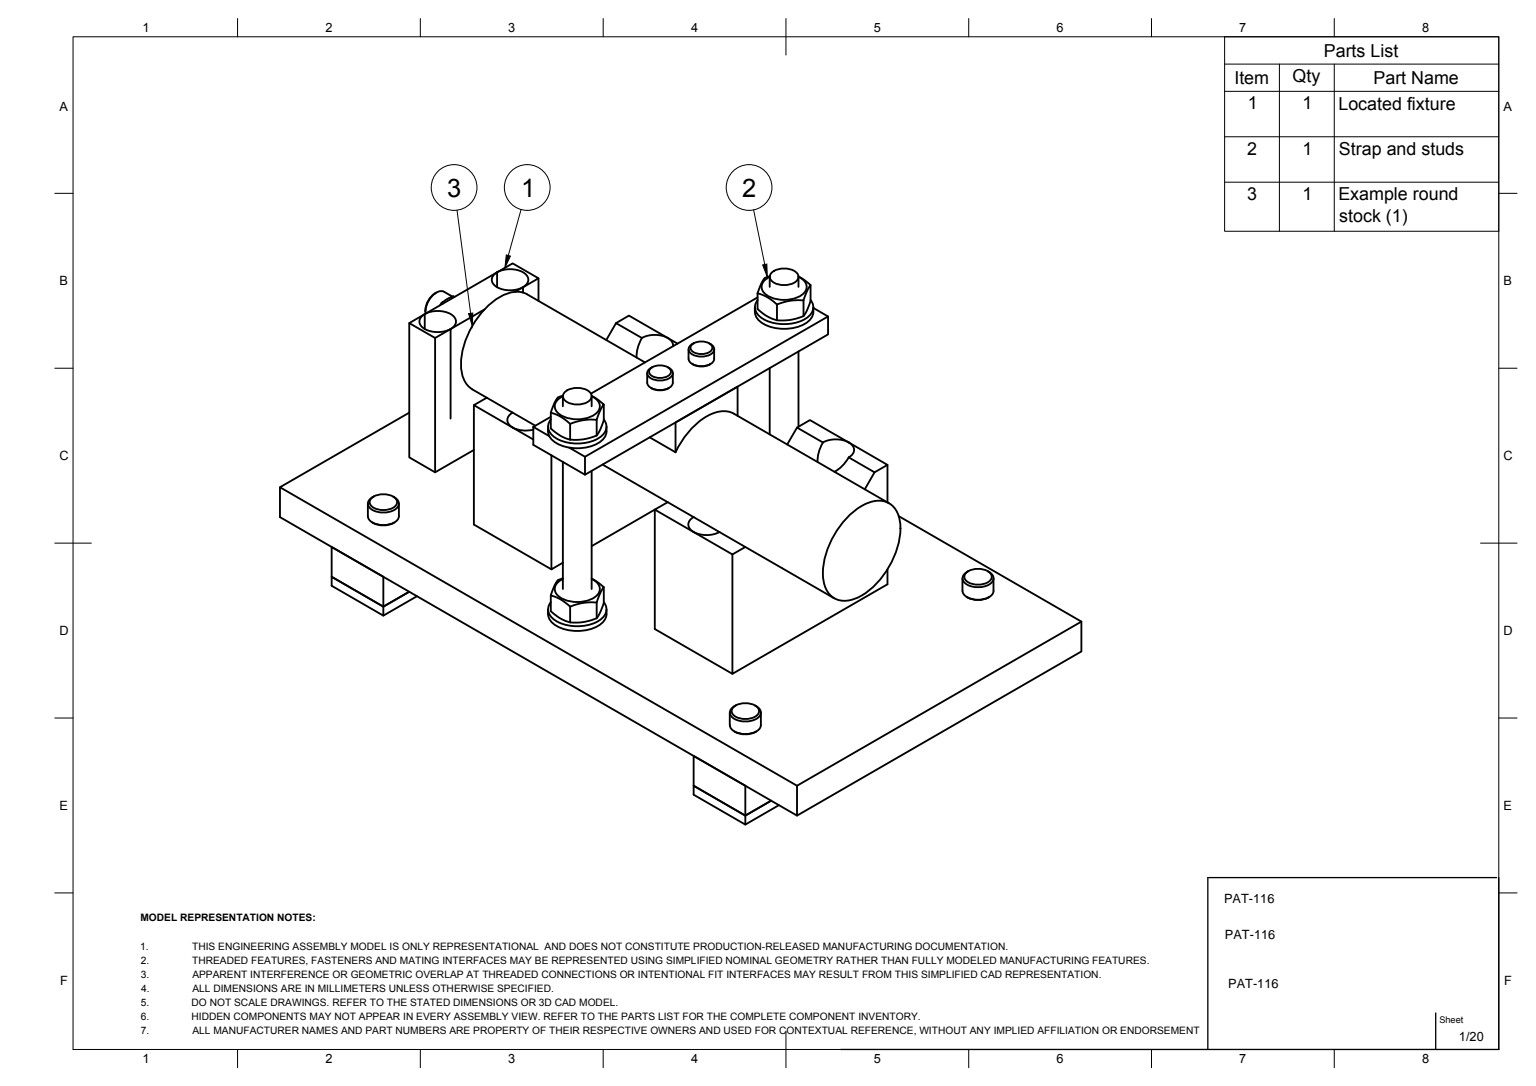
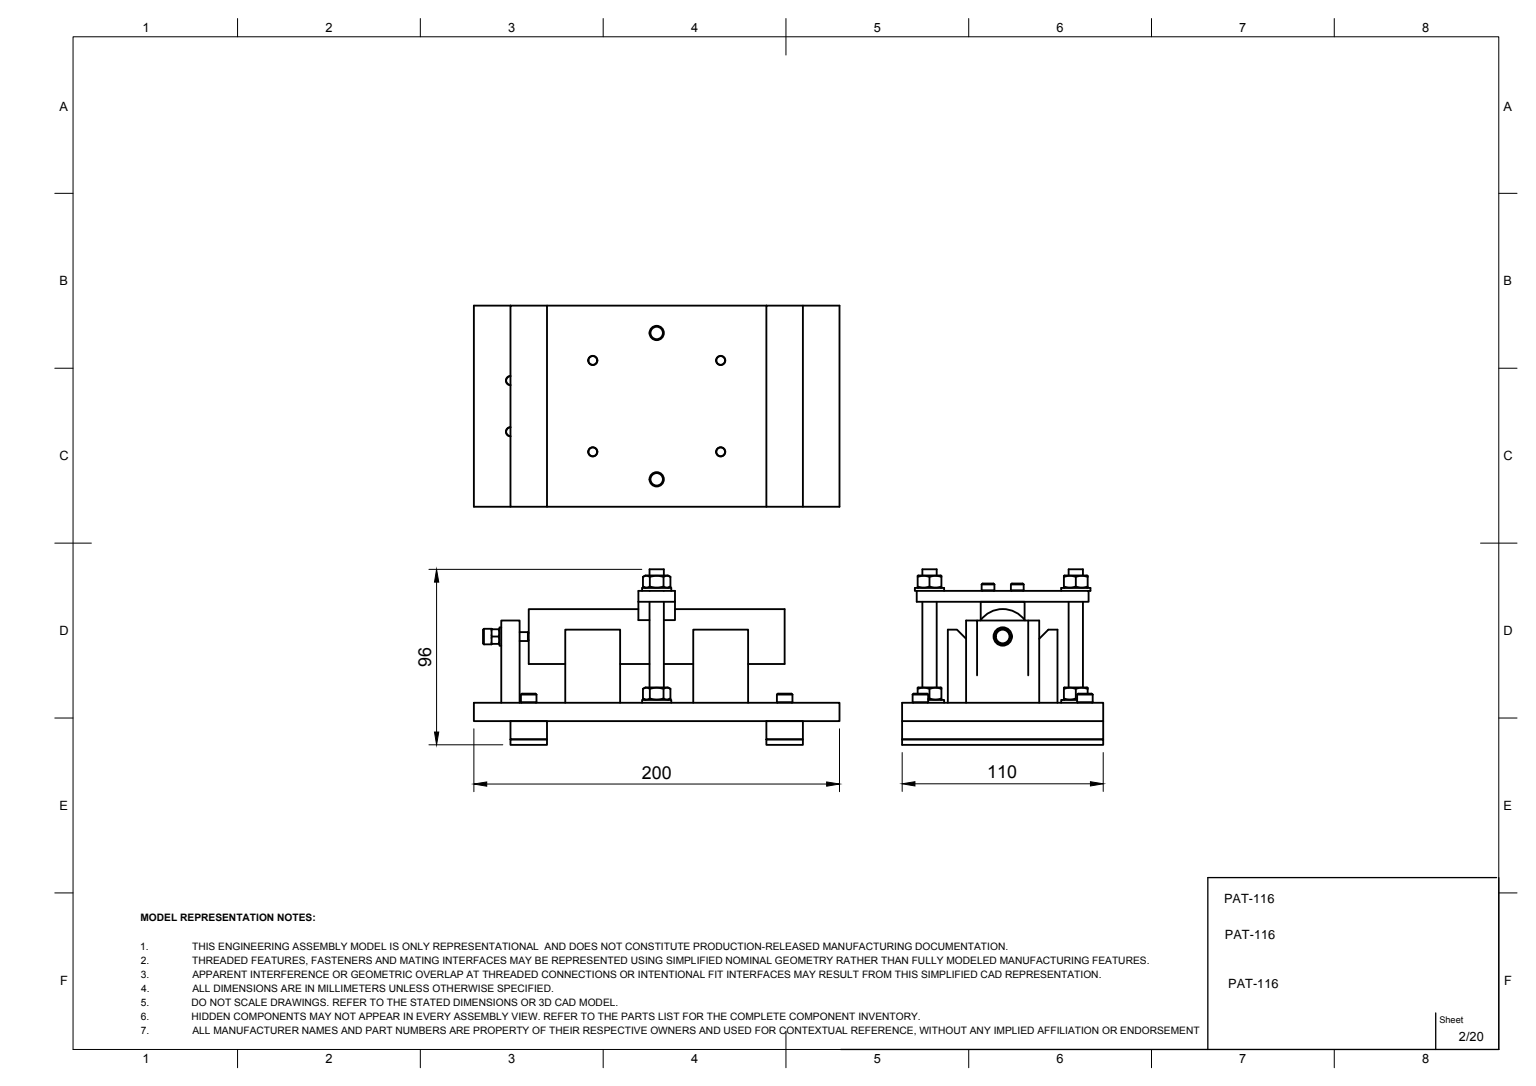
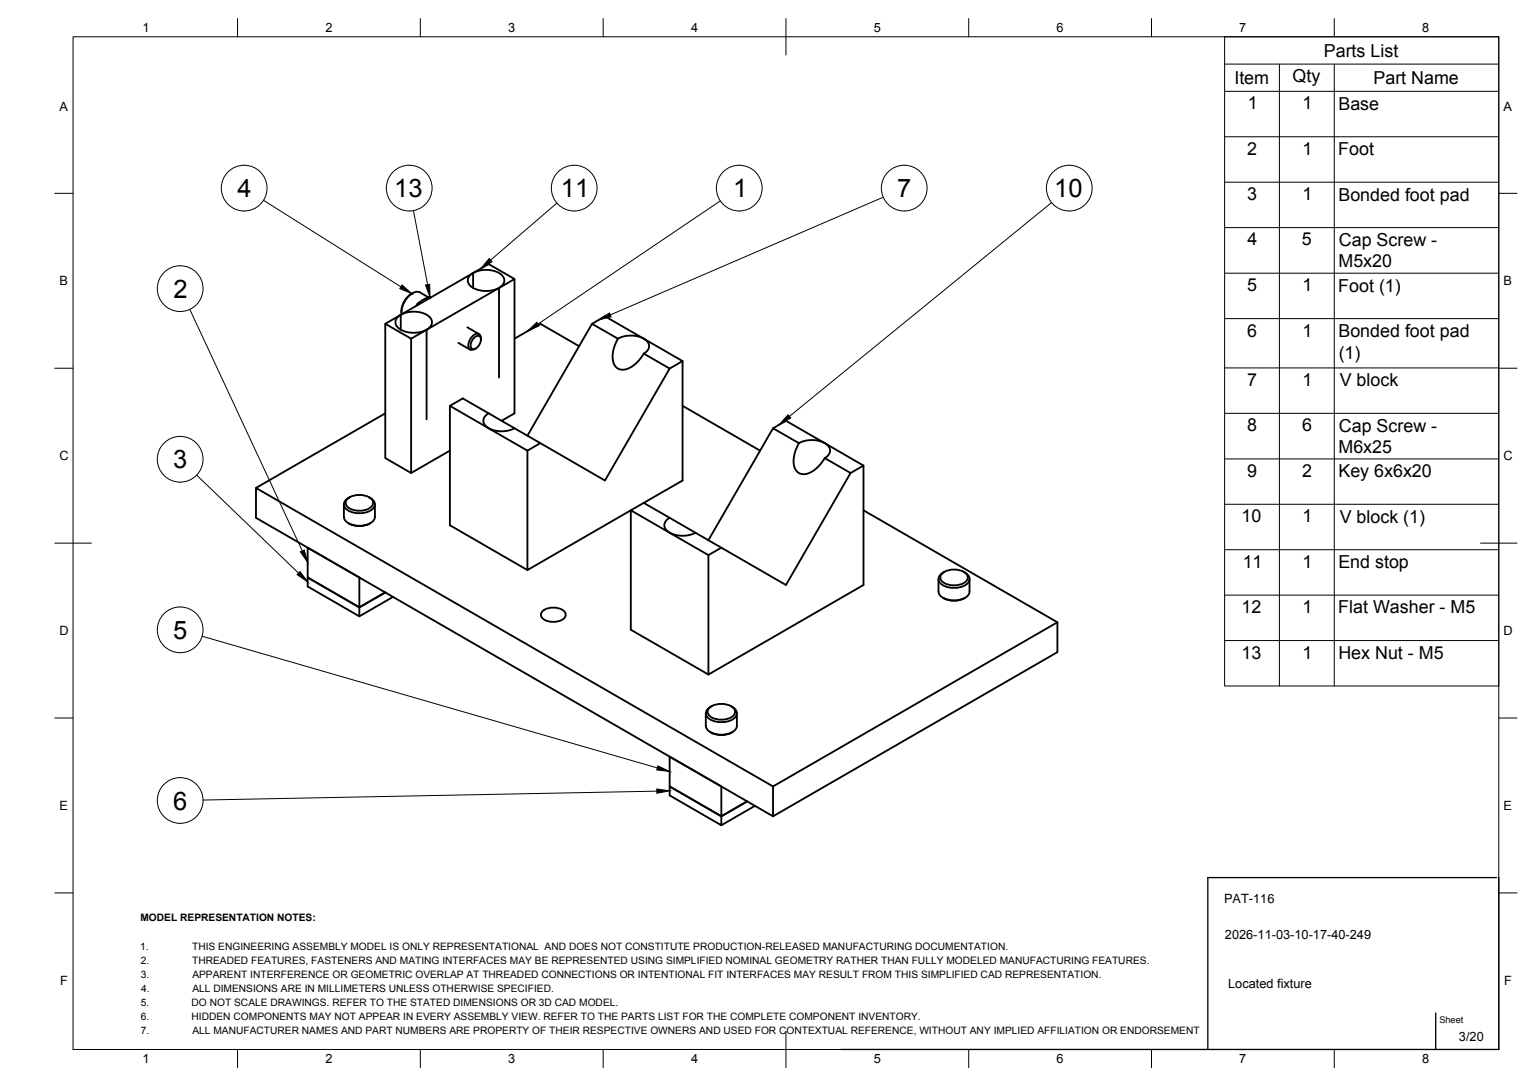
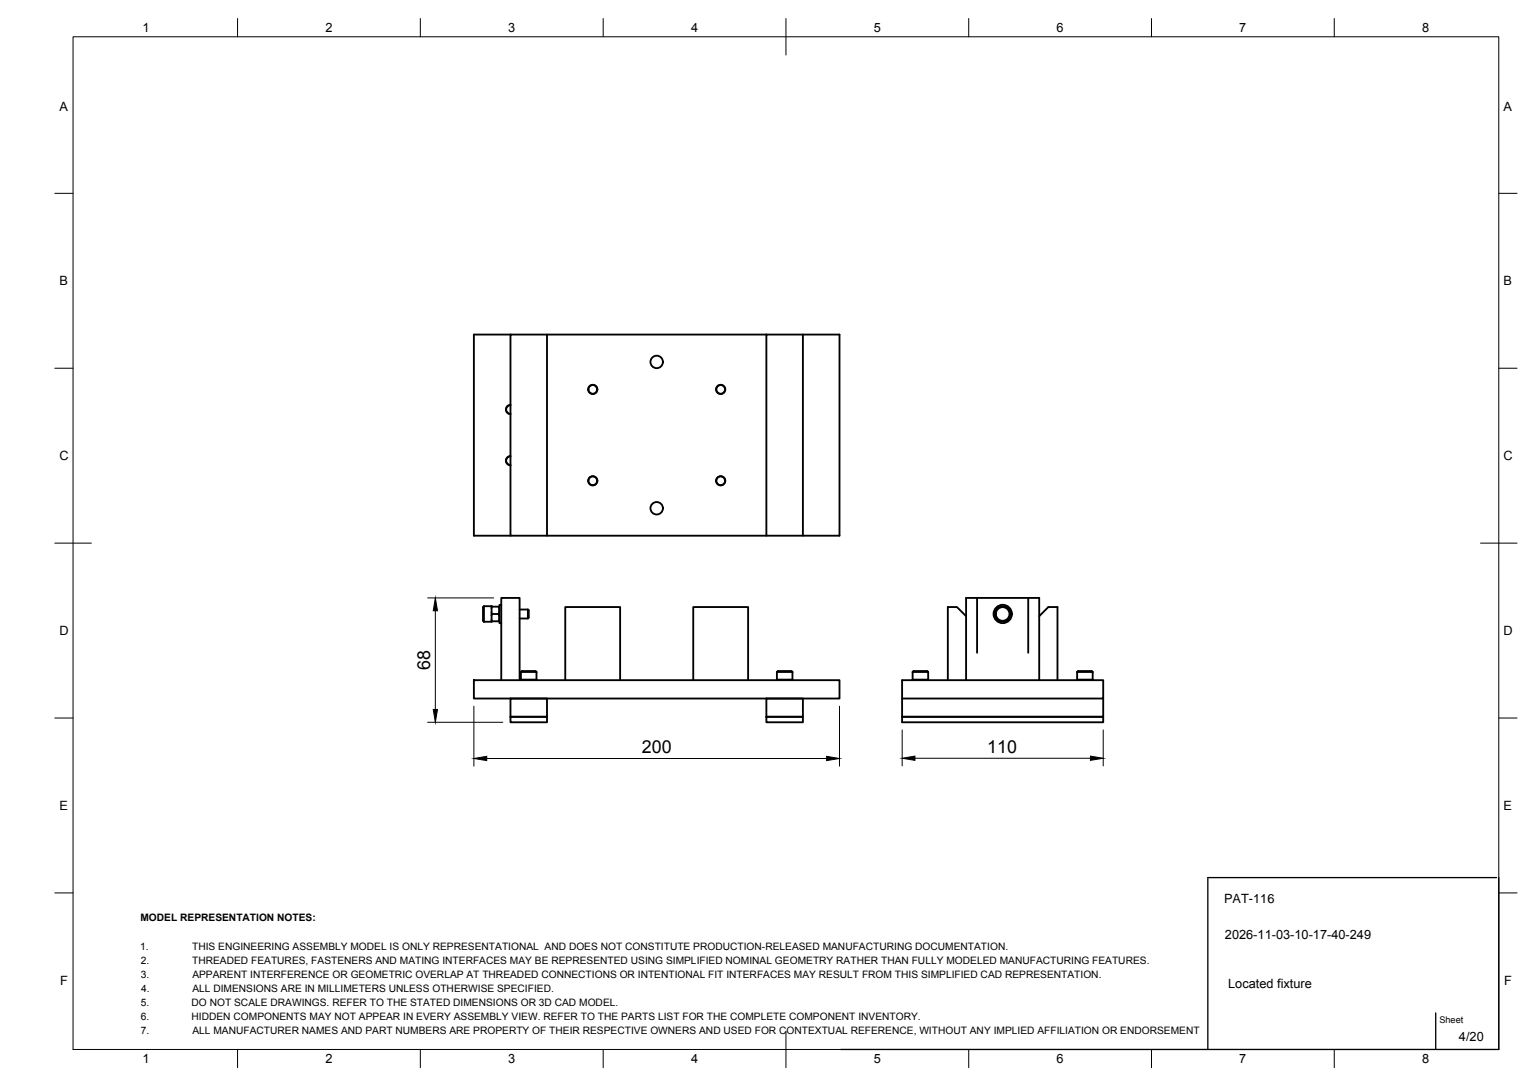
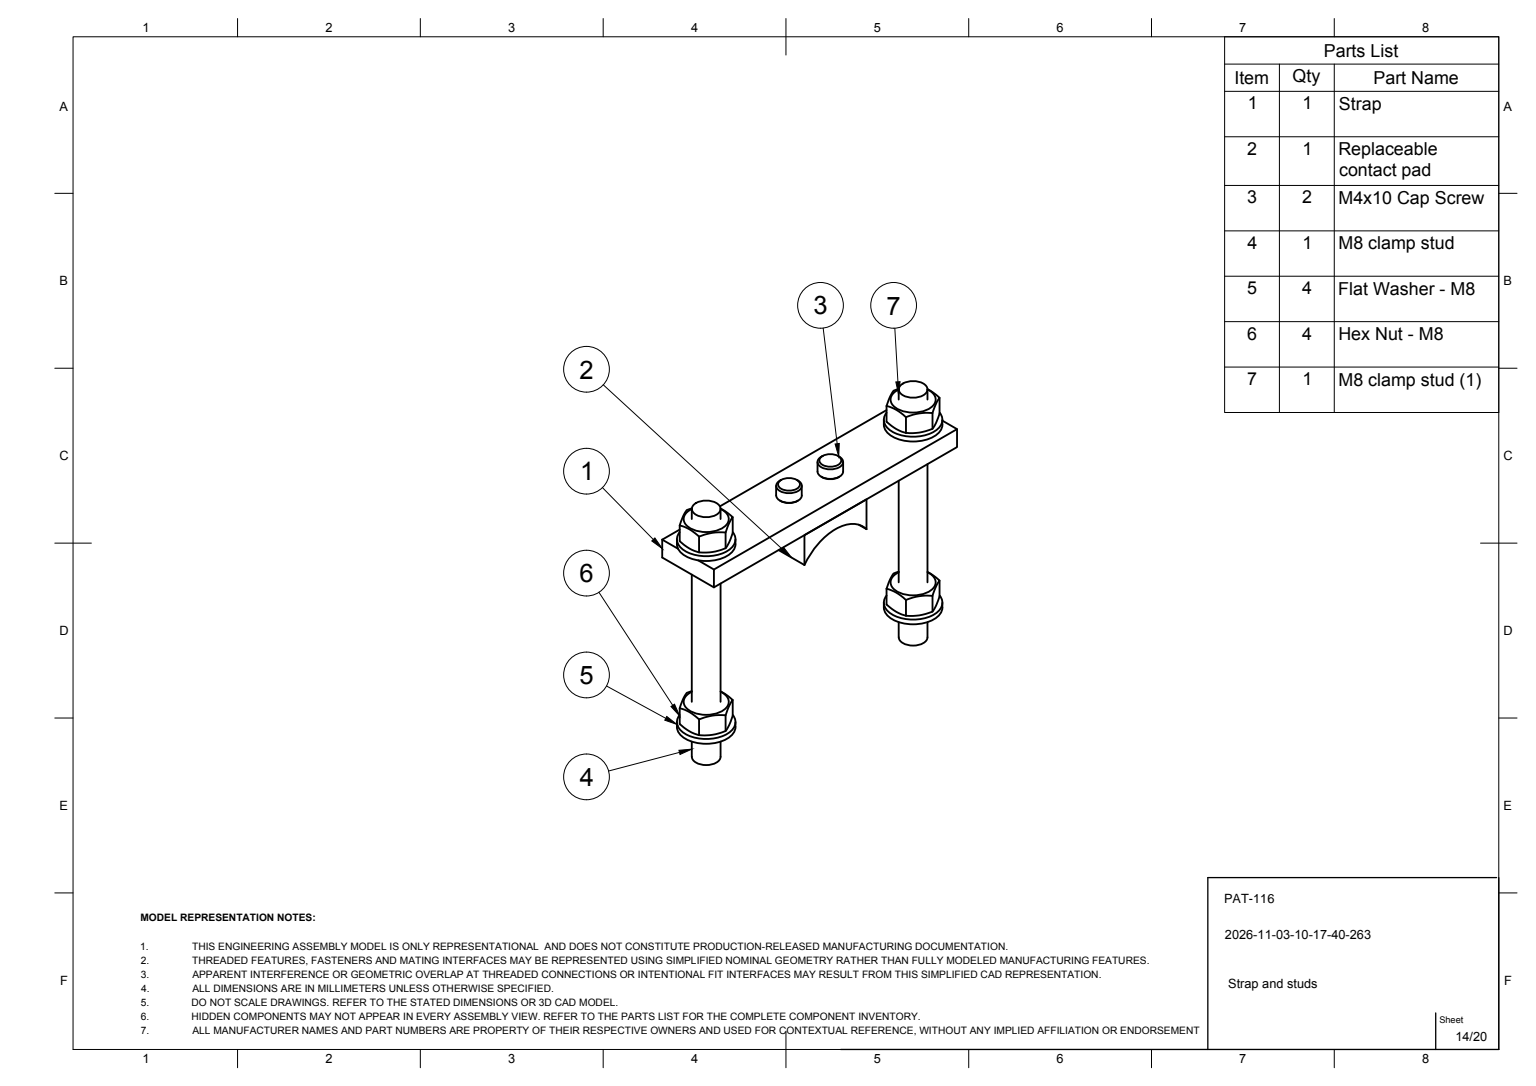
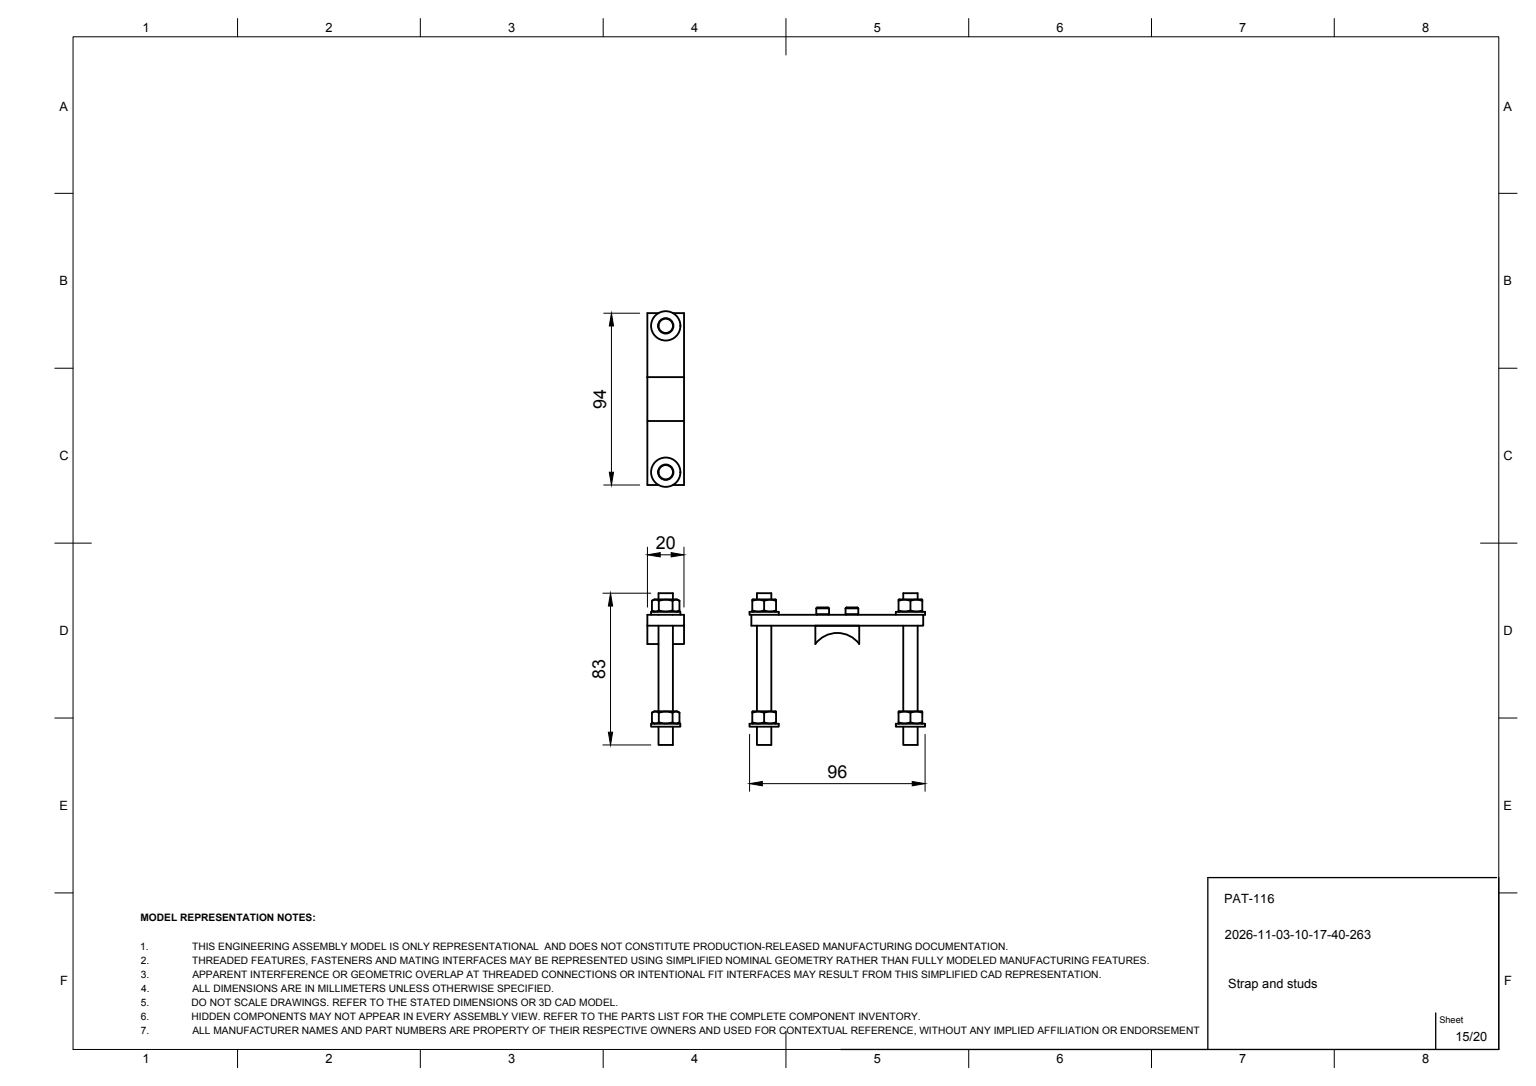
ISO-10303-21;
HEADER;
/* Generated by software containing ST-Developer
 * from STEP Tools, Inc. (www.steptools.com) 
 */

FILE_DESCRIPTION(
/* description */ ('V-block with clamp strap'),
/* implementation_level */ '2;1');

FILE_NAME(
/* name */ 'PAT-116',
/* time_stamp */ '2026-10-27T10:50:53-07:00',
/* author */ (''),
/* organization */ (''),
/* preprocessor_version */ 'ST-DEVELOPER v20.2',
/* originating_system */ 'Autodesk Translation Framework v15.17.0.0',
/* authorisation */ '');

FILE_SCHEMA (('AUTOMOTIVE_DESIGN { 1 0 10303 214 3 1 1 }'));
ENDSEC;

DATA;
#10=MECHANICAL_DESIGN_GEOMETRIC_PRESENTATION_REPRESENTATION('',(#266,#267,
#268,#269,#270,#271,#272,#273,#274,#275,#276,#277,#278,#279,#280,#281,#282,
#283,#284,#285,#286),#7344);
#11=ITEM_DEFINED_TRANSFORMATION($,$,#4406,#4697);
#12=ITEM_DEFINED_TRANSFORMATION($,$,#4459,#4698);
#13=ITEM_DEFINED_TRANSFORMATION($,$,#4472,#4699);
#14=ITEM_DEFINED_TRANSFORMATION($,$,#4479,#4700);
#15=ITEM_DEFINED_TRANSFORMATION($,$,#4492,#4701);
#16=ITEM_DEFINED_TRANSFORMATION($,$,#4499,#4702);
#17=ITEM_DEFINED_TRANSFORMATION($,$,#4538,#4703);
#18=ITEM_DEFINED_TRANSFORMATION($,$,#4577,#4704);
#19=ITEM_DEFINED_TRANSFORMATION($,$,#4646,#4705);
#20=ITEM_DEFINED_TRANSFORMATION($,$,#4646,#4706);
#21=ITEM_DEFINED_TRANSFORMATION($,$,#4646,#4707);
#22=ITEM_DEFINED_TRANSFORMATION($,$,#4646,#4708);
#23=ITEM_DEFINED_TRANSFORMATION($,$,#4620,#4709);
#24=ITEM_DEFINED_TRANSFORMATION($,$,#4620,#4710);
#25=ITEM_DEFINED_TRANSFORMATION($,$,#4609,#4711);
#26=ITEM_DEFINED_TRANSFORMATION($,$,#4620,#4712);
#27=ITEM_DEFINED_TRANSFORMATION($,$,#4620,#4713);
#28=ITEM_DEFINED_TRANSFORMATION($,$,#4609,#4714);
#29=ITEM_DEFINED_TRANSFORMATION($,$,#4620,#4715);
#30=ITEM_DEFINED_TRANSFORMATION($,$,#4620,#4716);
#31=ITEM_DEFINED_TRANSFORMATION($,$,#4646,#4717);
#32=ITEM_DEFINED_TRANSFORMATION($,$,#4672,#4718);
#33=ITEM_DEFINED_TRANSFORMATION($,$,#4681,#4719);
#34=ITEM_DEFINED_TRANSFORMATION($,$,#4721,#4818);
#35=ITEM_DEFINED_TRANSFORMATION($,$,#4740,#4819);
#36=ITEM_DEFINED_TRANSFORMATION($,$,#4757,#4820);
#37=ITEM_DEFINED_TRANSFORMATION($,$,#4763,#4821);
#38=ITEM_DEFINED_TRANSFORMATION($,$,#4769,#4822);
#39=ITEM_DEFINED_TRANSFORMATION($,$,#4769,#4823);
#40=ITEM_DEFINED_TRANSFORMATION($,$,#4793,#4824);
#41=ITEM_DEFINED_TRANSFORMATION($,$,#4802,#4825);
#42=ITEM_DEFINED_TRANSFORMATION($,$,#4793,#4826);
#43=ITEM_DEFINED_TRANSFORMATION($,$,#4802,#4827);
#44=ITEM_DEFINED_TRANSFORMATION($,$,#4793,#4828);
#45=ITEM_DEFINED_TRANSFORMATION($,$,#4802,#4829);
#46=ITEM_DEFINED_TRANSFORMATION($,$,#4793,#4830);
#47=ITEM_DEFINED_TRANSFORMATION($,$,#4802,#4831);
#48=ITEM_DEFINED_TRANSFORMATION($,$,#4833,#4839);
#49=ITEM_DEFINED_TRANSFORMATION($,$,#4405,#4840);
#50=ITEM_DEFINED_TRANSFORMATION($,$,#4720,#4841);
#51=ITEM_DEFINED_TRANSFORMATION($,$,#4832,#4842);
#52=(
REPRESENTATION_RELATIONSHIP($,$,#7442,#7441)
REPRESENTATION_RELATIONSHIP_WITH_TRANSFORMATION(#11)
SHAPE_REPRESENTATION_RELATIONSHIP()
);
#53=(
REPRESENTATION_RELATIONSHIP($,$,#7443,#7441)
REPRESENTATION_RELATIONSHIP_WITH_TRANSFORMATION(#12)
SHAPE_REPRESENTATION_RELATIONSHIP()
);
#54=(
REPRESENTATION_RELATIONSHIP($,$,#7444,#7441)
REPRESENTATION_RELATIONSHIP_WITH_TRANSFORMATION(#13)
SHAPE_REPRESENTATION_RELATIONSHIP()
);
#55=(
REPRESENTATION_RELATIONSHIP($,$,#7445,#7441)
REPRESENTATION_RELATIONSHIP_WITH_TRANSFORMATION(#14)
SHAPE_REPRESENTATION_RELATIONSHIP()
);
#56=(
REPRESENTATION_RELATIONSHIP($,$,#7446,#7441)
REPRESENTATION_RELATIONSHIP_WITH_TRANSFORMATION(#15)
SHAPE_REPRESENTATION_RELATIONSHIP()
);
#57=(
REPRESENTATION_RELATIONSHIP($,$,#7447,#7441)
REPRESENTATION_RELATIONSHIP_WITH_TRANSFORMATION(#16)
SHAPE_REPRESENTATION_RELATIONSHIP()
);
#58=(
REPRESENTATION_RELATIONSHIP($,$,#7448,#7441)
REPRESENTATION_RELATIONSHIP_WITH_TRANSFORMATION(#17)
SHAPE_REPRESENTATION_RELATIONSHIP()
);
#59=(
REPRESENTATION_RELATIONSHIP($,$,#7449,#7441)
REPRESENTATION_RELATIONSHIP_WITH_TRANSFORMATION(#18)
SHAPE_REPRESENTATION_RELATIONSHIP()
);
#60=(
REPRESENTATION_RELATIONSHIP($,$,#7452,#7441)
REPRESENTATION_RELATIONSHIP_WITH_TRANSFORMATION(#19)
SHAPE_REPRESENTATION_RELATIONSHIP()
);
#61=(
REPRESENTATION_RELATIONSHIP($,$,#7452,#7441)
REPRESENTATION_RELATIONSHIP_WITH_TRANSFORMATION(#20)
SHAPE_REPRESENTATION_RELATIONSHIP()
);
#62=(
REPRESENTATION_RELATIONSHIP($,$,#7452,#7441)
REPRESENTATION_RELATIONSHIP_WITH_TRANSFORMATION(#21)
SHAPE_REPRESENTATION_RELATIONSHIP()
);
#63=(
REPRESENTATION_RELATIONSHIP($,$,#7452,#7441)
REPRESENTATION_RELATIONSHIP_WITH_TRANSFORMATION(#22)
SHAPE_REPRESENTATION_RELATIONSHIP()
);
#64=(
REPRESENTATION_RELATIONSHIP($,$,#7451,#7441)
REPRESENTATION_RELATIONSHIP_WITH_TRANSFORMATION(#23)
SHAPE_REPRESENTATION_RELATIONSHIP()
);
#65=(
REPRESENTATION_RELATIONSHIP($,$,#7451,#7441)
REPRESENTATION_RELATIONSHIP_WITH_TRANSFORMATION(#24)
SHAPE_REPRESENTATION_RELATIONSHIP()
);
#66=(
REPRESENTATION_RELATIONSHIP($,$,#7450,#7441)
REPRESENTATION_RELATIONSHIP_WITH_TRANSFORMATION(#25)
SHAPE_REPRESENTATION_RELATIONSHIP()
);
#67=(
REPRESENTATION_RELATIONSHIP($,$,#7451,#7441)
REPRESENTATION_RELATIONSHIP_WITH_TRANSFORMATION(#26)
SHAPE_REPRESENTATION_RELATIONSHIP()
);
#68=(
REPRESENTATION_RELATIONSHIP($,$,#7451,#7441)
REPRESENTATION_RELATIONSHIP_WITH_TRANSFORMATION(#27)
SHAPE_REPRESENTATION_RELATIONSHIP()
);
#69=(
REPRESENTATION_RELATIONSHIP($,$,#7450,#7441)
REPRESENTATION_RELATIONSHIP_WITH_TRANSFORMATION(#28)
SHAPE_REPRESENTATION_RELATIONSHIP()
);
#70=(
REPRESENTATION_RELATIONSHIP($,$,#7451,#7441)
REPRESENTATION_RELATIONSHIP_WITH_TRANSFORMATION(#29)
SHAPE_REPRESENTATION_RELATIONSHIP()
);
#71=(
REPRESENTATION_RELATIONSHIP($,$,#7451,#7441)
REPRESENTATION_RELATIONSHIP_WITH_TRANSFORMATION(#30)
SHAPE_REPRESENTATION_RELATIONSHIP()
);
#72=(
REPRESENTATION_RELATIONSHIP($,$,#7452,#7441)
REPRESENTATION_RELATIONSHIP_WITH_TRANSFORMATION(#31)
SHAPE_REPRESENTATION_RELATIONSHIP()
);
#73=(
REPRESENTATION_RELATIONSHIP($,$,#7453,#7441)
REPRESENTATION_RELATIONSHIP_WITH_TRANSFORMATION(#32)
SHAPE_REPRESENTATION_RELATIONSHIP()
);
#74=(
REPRESENTATION_RELATIONSHIP($,$,#7454,#7441)
REPRESENTATION_RELATIONSHIP_WITH_TRANSFORMATION(#33)
SHAPE_REPRESENTATION_RELATIONSHIP()
);
#75=(
REPRESENTATION_RELATIONSHIP($,$,#7456,#7455)
REPRESENTATION_RELATIONSHIP_WITH_TRANSFORMATION(#34)
SHAPE_REPRESENTATION_RELATIONSHIP()
);
#76=(
REPRESENTATION_RELATIONSHIP($,$,#7457,#7455)
REPRESENTATION_RELATIONSHIP_WITH_TRANSFORMATION(#35)
SHAPE_REPRESENTATION_RELATIONSHIP()
);
#77=(
REPRESENTATION_RELATIONSHIP($,$,#7458,#7455)
REPRESENTATION_RELATIONSHIP_WITH_TRANSFORMATION(#36)
SHAPE_REPRESENTATION_RELATIONSHIP()
);
#78=(
REPRESENTATION_RELATIONSHIP($,$,#7459,#7455)
REPRESENTATION_RELATIONSHIP_WITH_TRANSFORMATION(#37)
SHAPE_REPRESENTATION_RELATIONSHIP()
);
#79=(
REPRESENTATION_RELATIONSHIP($,$,#7460,#7455)
REPRESENTATION_RELATIONSHIP_WITH_TRANSFORMATION(#38)
SHAPE_REPRESENTATION_RELATIONSHIP()
);
#80=(
REPRESENTATION_RELATIONSHIP($,$,#7460,#7455)
REPRESENTATION_RELATIONSHIP_WITH_TRANSFORMATION(#39)
SHAPE_REPRESENTATION_RELATIONSHIP()
);
#81=(
REPRESENTATION_RELATIONSHIP($,$,#7461,#7455)
REPRESENTATION_RELATIONSHIP_WITH_TRANSFORMATION(#40)
SHAPE_REPRESENTATION_RELATIONSHIP()
);
#82=(
REPRESENTATION_RELATIONSHIP($,$,#7462,#7455)
REPRESENTATION_RELATIONSHIP_WITH_TRANSFORMATION(#41)
SHAPE_REPRESENTATION_RELATIONSHIP()
);
#83=(
REPRESENTATION_RELATIONSHIP($,$,#7461,#7455)
REPRESENTATION_RELATIONSHIP_WITH_TRANSFORMATION(#42)
SHAPE_REPRESENTATION_RELATIONSHIP()
);
#84=(
REPRESENTATION_RELATIONSHIP($,$,#7462,#7455)
REPRESENTATION_RELATIONSHIP_WITH_TRANSFORMATION(#43)
SHAPE_REPRESENTATION_RELATIONSHIP()
);
#85=(
REPRESENTATION_RELATIONSHIP($,$,#7461,#7455)
REPRESENTATION_RELATIONSHIP_WITH_TRANSFORMATION(#44)
SHAPE_REPRESENTATION_RELATIONSHIP()
);
#86=(
REPRESENTATION_RELATIONSHIP($,$,#7462,#7455)
REPRESENTATION_RELATIONSHIP_WITH_TRANSFORMATION(#45)
SHAPE_REPRESENTATION_RELATIONSHIP()
);
#87=(
REPRESENTATION_RELATIONSHIP($,$,#7461,#7455)
REPRESENTATION_RELATIONSHIP_WITH_TRANSFORMATION(#46)
SHAPE_REPRESENTATION_RELATIONSHIP()
);
#88=(
REPRESENTATION_RELATIONSHIP($,$,#7462,#7455)
REPRESENTATION_RELATIONSHIP_WITH_TRANSFORMATION(#47)
SHAPE_REPRESENTATION_RELATIONSHIP()
);
#89=(
REPRESENTATION_RELATIONSHIP($,$,#7464,#7463)
REPRESENTATION_RELATIONSHIP_WITH_TRANSFORMATION(#48)
SHAPE_REPRESENTATION_RELATIONSHIP()
);
#90=(
REPRESENTATION_RELATIONSHIP($,$,#7441,#7440)
REPRESENTATION_RELATIONSHIP_WITH_TRANSFORMATION(#49)
SHAPE_REPRESENTATION_RELATIONSHIP()
);
#91=(
REPRESENTATION_RELATIONSHIP($,$,#7455,#7440)
REPRESENTATION_RELATIONSHIP_WITH_TRANSFORMATION(#50)
SHAPE_REPRESENTATION_RELATIONSHIP()
);
#92=(
REPRESENTATION_RELATIONSHIP($,$,#7463,#7440)
REPRESENTATION_RELATIONSHIP_WITH_TRANSFORMATION(#51)
SHAPE_REPRESENTATION_RELATIONSHIP()
);
#93=CONTEXT_DEPENDENT_SHAPE_REPRESENTATION(#52,#7389);
#94=CONTEXT_DEPENDENT_SHAPE_REPRESENTATION(#53,#7390);
#95=CONTEXT_DEPENDENT_SHAPE_REPRESENTATION(#54,#7391);
#96=CONTEXT_DEPENDENT_SHAPE_REPRESENTATION(#55,#7392);
#97=CONTEXT_DEPENDENT_SHAPE_REPRESENTATION(#56,#7393);
#98=CONTEXT_DEPENDENT_SHAPE_REPRESENTATION(#57,#7394);
#99=CONTEXT_DEPENDENT_SHAPE_REPRESENTATION(#58,#7395);
#100=CONTEXT_DEPENDENT_SHAPE_REPRESENTATION(#59,#7396);
#101=CONTEXT_DEPENDENT_SHAPE_REPRESENTATION(#60,#7397);
#102=CONTEXT_DEPENDENT_SHAPE_REPRESENTATION(#61,#7398);
#103=CONTEXT_DEPENDENT_SHAPE_REPRESENTATION(#62,#7399);
#104=CONTEXT_DEPENDENT_SHAPE_REPRESENTATION(#63,#7400);
#105=CONTEXT_DEPENDENT_SHAPE_REPRESENTATION(#64,#7401);
#106=CONTEXT_DEPENDENT_SHAPE_REPRESENTATION(#65,#7402);
#107=CONTEXT_DEPENDENT_SHAPE_REPRESENTATION(#66,#7403);
#108=CONTEXT_DEPENDENT_SHAPE_REPRESENTATION(#67,#7404);
#109=CONTEXT_DEPENDENT_SHAPE_REPRESENTATION(#68,#7405);
#110=CONTEXT_DEPENDENT_SHAPE_REPRESENTATION(#69,#7406);
#111=CONTEXT_DEPENDENT_SHAPE_REPRESENTATION(#70,#7407);
#112=CONTEXT_DEPENDENT_SHAPE_REPRESENTATION(#71,#7408);
#113=CONTEXT_DEPENDENT_SHAPE_REPRESENTATION(#72,#7409);
#114=CONTEXT_DEPENDENT_SHAPE_REPRESENTATION(#73,#7410);
#115=CONTEXT_DEPENDENT_SHAPE_REPRESENTATION(#74,#7411);
#116=CONTEXT_DEPENDENT_SHAPE_REPRESENTATION(#75,#7420);
#117=CONTEXT_DEPENDENT_SHAPE_REPRESENTATION(#76,#7421);
#118=CONTEXT_DEPENDENT_SHAPE_REPRESENTATION(#77,#7422);
#119=CONTEXT_DEPENDENT_SHAPE_REPRESENTATION(#78,#7423);
#120=CONTEXT_DEPENDENT_SHAPE_REPRESENTATION(#79,#7424);
#121=CONTEXT_DEPENDENT_SHAPE_REPRESENTATION(#80,#7425);
#122=CONTEXT_DEPENDENT_SHAPE_REPRESENTATION(#81,#7426);
#123=CONTEXT_DEPENDENT_SHAPE_REPRESENTATION(#82,#7427);
#124=CONTEXT_DEPENDENT_SHAPE_REPRESENTATION(#83,#7428);
#125=CONTEXT_DEPENDENT_SHAPE_REPRESENTATION(#84,#7429);
#126=CONTEXT_DEPENDENT_SHAPE_REPRESENTATION(#85,#7430);
#127=CONTEXT_DEPENDENT_SHAPE_REPRESENTATION(#86,#7431);
#128=CONTEXT_DEPENDENT_SHAPE_REPRESENTATION(#87,#7432);
#129=CONTEXT_DEPENDENT_SHAPE_REPRESENTATION(#88,#7433);
#130=CONTEXT_DEPENDENT_SHAPE_REPRESENTATION(#89,#7436);
#131=CONTEXT_DEPENDENT_SHAPE_REPRESENTATION(#90,#7437);
#132=CONTEXT_DEPENDENT_SHAPE_REPRESENTATION(#91,#7438);
#133=CONTEXT_DEPENDENT_SHAPE_REPRESENTATION(#92,#7439);
#134=NEXT_ASSEMBLY_USAGE_OCCURRENCE('Base:1','Base:1','Base:1',#7467,#7468,
'Base:1');
#135=NEXT_ASSEMBLY_USAGE_OCCURRENCE('Foot:1','Foot:1','Foot:1',#7467,#7469,
'Foot:1');
#136=NEXT_ASSEMBLY_USAGE_OCCURRENCE('Bonded foot pad:1',
'Bonded foot pad:1','Bonded foot pad:1',#7467,#7470,'Bonded foot pad:1');
#137=NEXT_ASSEMBLY_USAGE_OCCURRENCE('Foot (1):1','Foot (1):1',
'Foot (1):1',#7467,#7471,'Foot (1):1');
#138=NEXT_ASSEMBLY_USAGE_OCCURRENCE('Bonded foot pad (1):1',
'Bonded foot pad (1):1','Bonded foot pad (1):1',#7467,#7472,
'Bonded foot pad (1):1');
#139=NEXT_ASSEMBLY_USAGE_OCCURRENCE('V block:1','V block:1','V block:1',
#7467,#7473,'V block:1');
#140=NEXT_ASSEMBLY_USAGE_OCCURRENCE('V block (1):1','V block (1):1',
'V block (1):1',#7467,#7474,'V block (1):1');
#141=NEXT_ASSEMBLY_USAGE_OCCURRENCE('End stop:1','End stop:1',
'End stop:1',#7467,#7475,'End stop:1');
#142=NEXT_ASSEMBLY_USAGE_OCCURRENCE('Cap Screw - M5x20:2',
'Cap Screw - M5x20:2','Cap Screw - M5x20:2',#7467,#7478,
'Cap Screw - M5x20:2');
#143=NEXT_ASSEMBLY_USAGE_OCCURRENCE('Cap Screw - M5x20:3',
'Cap Screw - M5x20:3','Cap Screw - M5x20:3',#7467,#7478,
'Cap Screw - M5x20:3');
#144=NEXT_ASSEMBLY_USAGE_OCCURRENCE('Cap Screw - M5x20:4',
'Cap Screw - M5x20:4','Cap Screw - M5x20:4',#7467,#7478,
'Cap Screw - M5x20:4');
#145=NEXT_ASSEMBLY_USAGE_OCCURRENCE('Cap Screw - M5x20:5',
'Cap Screw - M5x20:5','Cap Screw - M5x20:5',#7467,#7478,
'Cap Screw - M5x20:5');
#146=NEXT_ASSEMBLY_USAGE_OCCURRENCE('Cap Screw - M6x25:2',
'Cap Screw - M6x25:2','Cap Screw - M6x25:2',#7467,#7477,
'Cap Screw - M6x25:2');
#147=NEXT_ASSEMBLY_USAGE_OCCURRENCE('Cap Screw - M6x25:3',
'Cap Screw - M6x25:3','Cap Screw - M6x25:3',#7467,#7477,
'Cap Screw - M6x25:3');
#148=NEXT_ASSEMBLY_USAGE_OCCURRENCE('Key 6x6x20:2','Key 6x6x20:2',
'Key 6x6x20:2',#7467,#7476,'Key 6x6x20:2');
#149=NEXT_ASSEMBLY_USAGE_OCCURRENCE('Cap Screw - M6x25:4',
'Cap Screw - M6x25:4','Cap Screw - M6x25:4',#7467,#7477,
'Cap Screw - M6x25:4');
#150=NEXT_ASSEMBLY_USAGE_OCCURRENCE('Cap Screw - M6x25:5',
'Cap Screw - M6x25:5','Cap Screw - M6x25:5',#7467,#7477,
'Cap Screw - M6x25:5');
#151=NEXT_ASSEMBLY_USAGE_OCCURRENCE('Key 6x6x20:3','Key 6x6x20:3',
'Key 6x6x20:3',#7467,#7476,'Key 6x6x20:3');
#152=NEXT_ASSEMBLY_USAGE_OCCURRENCE('Cap Screw - M6x25:6',
'Cap Screw - M6x25:6','Cap Screw - M6x25:6',#7467,#7477,
'Cap Screw - M6x25:6');
#153=NEXT_ASSEMBLY_USAGE_OCCURRENCE('Cap Screw - M6x25:7',
'Cap Screw - M6x25:7','Cap Screw - M6x25:7',#7467,#7477,
'Cap Screw - M6x25:7');
#154=NEXT_ASSEMBLY_USAGE_OCCURRENCE('Cap Screw - M5x20:6',
'Cap Screw - M5x20:6','Cap Screw - M5x20:6',#7467,#7478,
'Cap Screw - M5x20:6');
#155=NEXT_ASSEMBLY_USAGE_OCCURRENCE('Flat Washer - M5:2',
'Flat Washer - M5:2','Flat Washer - M5:2',#7467,#7479,
'Flat Washer - M5:2');
#156=NEXT_ASSEMBLY_USAGE_OCCURRENCE('Hex Nut - M5:2','Hex Nut - M5:2',
'Hex Nut - M5:2',#7467,#7480,'Hex Nut - M5:2');
#157=NEXT_ASSEMBLY_USAGE_OCCURRENCE('Strap:1','Strap:1','Strap:1',#7481,
#7482,'Strap:1');
#158=NEXT_ASSEMBLY_USAGE_OCCURRENCE('Replaceable contact pad:1',
'Replaceable contact pad:1','Replaceable contact pad:1',#7481,#7483,
'Replaceable contact pad:1');
#159=NEXT_ASSEMBLY_USAGE_OCCURRENCE('M8 clamp stud:1','M8 clamp stud:1',
'M8 clamp stud:1',#7481,#7484,'M8 clamp stud:1');
#160=NEXT_ASSEMBLY_USAGE_OCCURRENCE('M8 clamp stud (1):1',
'M8 clamp stud (1):1','M8 clamp stud (1):1',#7481,#7485,
'M8 clamp stud (1):1');
#161=NEXT_ASSEMBLY_USAGE_OCCURRENCE('M4x10 Cap Screw:2',
'M4x10 Cap Screw:2','M4x10 Cap Screw:2',#7481,#7486,'M4x10 Cap Screw:2');
#162=NEXT_ASSEMBLY_USAGE_OCCURRENCE('M4x10 Cap Screw:3',
'M4x10 Cap Screw:3','M4x10 Cap Screw:3',#7481,#7486,'M4x10 Cap Screw:3');
#163=NEXT_ASSEMBLY_USAGE_OCCURRENCE('Flat Washer - M8:2',
'Flat Washer - M8:2','Flat Washer - M8:2',#7481,#7487,
'Flat Washer - M8:2');
#164=NEXT_ASSEMBLY_USAGE_OCCURRENCE('Hex Nut - M8:2','Hex Nut - M8:2',
'Hex Nut - M8:2',#7481,#7488,'Hex Nut - M8:2');
#165=NEXT_ASSEMBLY_USAGE_OCCURRENCE('Flat Washer - M8:3',
'Flat Washer - M8:3','Flat Washer - M8:3',#7481,#7487,
'Flat Washer - M8:3');
#166=NEXT_ASSEMBLY_USAGE_OCCURRENCE('Hex Nut - M8:3','Hex Nut - M8:3',
'Hex Nut - M8:3',#7481,#7488,'Hex Nut - M8:3');
#167=NEXT_ASSEMBLY_USAGE_OCCURRENCE('Flat Washer - M8:4',
'Flat Washer - M8:4','Flat Washer - M8:4',#7481,#7487,
'Flat Washer - M8:4');
#168=NEXT_ASSEMBLY_USAGE_OCCURRENCE('Hex Nut - M8:4','Hex Nut - M8:4',
'Hex Nut - M8:4',#7481,#7488,'Hex Nut - M8:4');
#169=NEXT_ASSEMBLY_USAGE_OCCURRENCE('Flat Washer - M8:5',
'Flat Washer - M8:5','Flat Washer - M8:5',#7481,#7487,
'Flat Washer - M8:5');
#170=NEXT_ASSEMBLY_USAGE_OCCURRENCE('Hex Nut - M8:5','Hex Nut - M8:5',
'Hex Nut - M8:5',#7481,#7488,'Hex Nut - M8:5');
#171=NEXT_ASSEMBLY_USAGE_OCCURRENCE('Example round stock:1',
'Example round stock:1','Example round stock:1',#7489,#7490,
'Example round stock:1');
#172=NEXT_ASSEMBLY_USAGE_OCCURRENCE('Located fixture:1',
'Located fixture:1','Located fixture:1',#7466,#7467,'Located fixture:1');
#173=NEXT_ASSEMBLY_USAGE_OCCURRENCE('Strap and studs:1',
'Strap and studs:1','Strap and studs:1',#7466,#7481,'Strap and studs:1');
#174=NEXT_ASSEMBLY_USAGE_OCCURRENCE('Example round stock (1):1',
'Example round stock (1):1','Example round stock (1):1',#7466,#7489,
'Example round stock (1):1');
#175=(
BOUNDED_CURVE()
B_SPLINE_CURVE(2,(#6900,#6901,#6902),.UNSPECIFIED.,.F.,.F.)
B_SPLINE_CURVE_WITH_KNOTS((3,3),(0.140651836354967,0.670383167684795),
 .UNSPECIFIED.)
CURVE()
GEOMETRIC_REPRESENTATION_ITEM()
RATIONAL_B_SPLINE_CURVE((1.11602540378444,1.28867513459481,1.11602540378444))
REPRESENTATION_ITEM('')
);
#176=(
BOUNDED_CURVE()
B_SPLINE_CURVE(2,(#6904,#6905,#6906),.UNSPECIFIED.,.F.,.F.)
B_SPLINE_CURVE_WITH_KNOTS((3,3),(0.140651836354967,0.670383167684795),
 .UNSPECIFIED.)
CURVE()
GEOMETRIC_REPRESENTATION_ITEM()
RATIONAL_B_SPLINE_CURVE((1.11602540378444,1.28867513459481,1.11602540378444))
REPRESENTATION_ITEM('')
);
#177=(
BOUNDED_CURVE()
B_SPLINE_CURVE(2,(#6911,#6912,#6913),.UNSPECIFIED.,.F.,.F.)
B_SPLINE_CURVE_WITH_KNOTS((3,3),(0.140651836354967,0.670383167684795),
 .UNSPECIFIED.)
CURVE()
GEOMETRIC_REPRESENTATION_ITEM()
RATIONAL_B_SPLINE_CURVE((1.11602540378444,1.28867513459481,1.11602540378444))
REPRESENTATION_ITEM('')
);
#178=(
BOUNDED_CURVE()
B_SPLINE_CURVE(2,(#6915,#6916,#6917),.UNSPECIFIED.,.F.,.F.)
B_SPLINE_CURVE_WITH_KNOTS((3,3),(0.140651836354967,0.670383167684795),
 .UNSPECIFIED.)
CURVE()
GEOMETRIC_REPRESENTATION_ITEM()
RATIONAL_B_SPLINE_CURVE((1.11602540378444,1.28867513459481,1.11602540378444))
REPRESENTATION_ITEM('')
);
#179=(
BOUNDED_CURVE()
B_SPLINE_CURVE(2,(#6919,#6920,#6921),.UNSPECIFIED.,.F.,.F.)
B_SPLINE_CURVE_WITH_KNOTS((3,3),(0.140651836354967,0.670383167684795),
 .UNSPECIFIED.)
CURVE()
GEOMETRIC_REPRESENTATION_ITEM()
RATIONAL_B_SPLINE_CURVE((1.11602540378444,1.28867513459481,1.11602540378444))
REPRESENTATION_ITEM('')
);
#180=(
BOUNDED_CURVE()
B_SPLINE_CURVE(2,(#6922,#6923,#6924),.UNSPECIFIED.,.F.,.F.)
B_SPLINE_CURVE_WITH_KNOTS((3,3),(0.140651836354967,0.670383167684795),
 .UNSPECIFIED.)
CURVE()
GEOMETRIC_REPRESENTATION_ITEM()
RATIONAL_B_SPLINE_CURVE((1.11602540378444,1.28867513459481,1.11602540378444))
REPRESENTATION_ITEM('')
);
#181=(
BOUNDED_CURVE()
B_SPLINE_CURVE(2,(#6931,#6932,#6933),.UNSPECIFIED.,.F.,.F.)
B_SPLINE_CURVE_WITH_KNOTS((3,3),(0.140651836354967,0.670383167684795),
 .UNSPECIFIED.)
CURVE()
GEOMETRIC_REPRESENTATION_ITEM()
RATIONAL_B_SPLINE_CURVE((1.11602540378444,1.28867513459481,1.11602540378444))
REPRESENTATION_ITEM('')
);
#182=(
BOUNDED_CURVE()
B_SPLINE_CURVE(2,(#6935,#6936,#6937),.UNSPECIFIED.,.F.,.F.)
B_SPLINE_CURVE_WITH_KNOTS((3,3),(0.140651836354967,0.670383167684796),
 .UNSPECIFIED.)
CURVE()
GEOMETRIC_REPRESENTATION_ITEM()
RATIONAL_B_SPLINE_CURVE((1.11602540378444,1.28867513459481,1.11602540378444))
REPRESENTATION_ITEM('')
);
#183=(
BOUNDED_CURVE()
B_SPLINE_CURVE(2,(#6939,#6940,#6941),.UNSPECIFIED.,.F.,.F.)
B_SPLINE_CURVE_WITH_KNOTS((3,3),(0.140651836354967,0.670383167684795),
 .UNSPECIFIED.)
CURVE()
GEOMETRIC_REPRESENTATION_ITEM()
RATIONAL_B_SPLINE_CURVE((1.11602540378444,1.28867513459481,1.11602540378444))
REPRESENTATION_ITEM('')
);
#184=(
BOUNDED_CURVE()
B_SPLINE_CURVE(2,(#6943,#6944,#6945),.UNSPECIFIED.,.F.,.F.)
B_SPLINE_CURVE_WITH_KNOTS((3,3),(0.140651836354967,0.670383167684795),
 .UNSPECIFIED.)
CURVE()
GEOMETRIC_REPRESENTATION_ITEM()
RATIONAL_B_SPLINE_CURVE((1.11602540378444,1.28867513459482,1.11602540378444))
REPRESENTATION_ITEM('')
);
#185=(
BOUNDED_CURVE()
B_SPLINE_CURVE(2,(#6947,#6948,#6949),.UNSPECIFIED.,.F.,.F.)
B_SPLINE_CURVE_WITH_KNOTS((3,3),(0.140651836354967,0.670383167684795),
 .UNSPECIFIED.)
CURVE()
GEOMETRIC_REPRESENTATION_ITEM()
RATIONAL_B_SPLINE_CURVE((1.11602540378444,1.28867513459481,1.11602540378444))
REPRESENTATION_ITEM('')
);
#186=(
BOUNDED_CURVE()
B_SPLINE_CURVE(2,(#6950,#6951,#6952),.UNSPECIFIED.,.F.,.F.)
B_SPLINE_CURVE_WITH_KNOTS((3,3),(0.140651836354967,0.670383167684795),
 .UNSPECIFIED.)
CURVE()
GEOMETRIC_REPRESENTATION_ITEM()
RATIONAL_B_SPLINE_CURVE((1.11602540378444,1.28867513459481,1.11602540378444))
REPRESENTATION_ITEM('')
);
#187=(
BOUNDED_CURVE()
B_SPLINE_CURVE(2,(#7192,#7193,#7194),.UNSPECIFIED.,.F.,.F.)
B_SPLINE_CURVE_WITH_KNOTS((3,3),(0.14973948338295,0.97160236658079),
 .UNSPECIFIED.)
CURVE()
GEOMETRIC_REPRESENTATION_ITEM()
RATIONAL_B_SPLINE_CURVE((1.07140024848292,1.23714644374248,1.07140024848292))
REPRESENTATION_ITEM('')
);
#188=(
BOUNDED_CURVE()
B_SPLINE_CURVE(2,(#7196,#7197,#7198),.UNSPECIFIED.,.F.,.F.)
B_SPLINE_CURVE_WITH_KNOTS((3,3),(0.14973948338295,0.971602366580789),
 .UNSPECIFIED.)
CURVE()
GEOMETRIC_REPRESENTATION_ITEM()
RATIONAL_B_SPLINE_CURVE((1.07140024848292,1.23714644374248,1.07140024848292))
REPRESENTATION_ITEM('')
);
#189=(
BOUNDED_CURVE()
B_SPLINE_CURVE(2,(#7203,#7204,#7205),.UNSPECIFIED.,.F.,.F.)
B_SPLINE_CURVE_WITH_KNOTS((3,3),(0.14973948338295,0.97160236658079),
 .UNSPECIFIED.)
CURVE()
GEOMETRIC_REPRESENTATION_ITEM()
RATIONAL_B_SPLINE_CURVE((1.07140024848292,1.23714644374248,1.07140024848292))
REPRESENTATION_ITEM('')
);
#190=(
BOUNDED_CURVE()
B_SPLINE_CURVE(2,(#7207,#7208,#7209),.UNSPECIFIED.,.F.,.F.)
B_SPLINE_CURVE_WITH_KNOTS((3,3),(0.14973948338295,0.97160236658079),
 .UNSPECIFIED.)
CURVE()
GEOMETRIC_REPRESENTATION_ITEM()
RATIONAL_B_SPLINE_CURVE((1.07140024848292,1.23714644374248,1.07140024848292))
REPRESENTATION_ITEM('')
);
#191=(
BOUNDED_CURVE()
B_SPLINE_CURVE(2,(#7211,#7212,#7213),.UNSPECIFIED.,.F.,.F.)
B_SPLINE_CURVE_WITH_KNOTS((3,3),(0.14973948338295,0.971602366580789),
 .UNSPECIFIED.)
CURVE()
GEOMETRIC_REPRESENTATION_ITEM()
RATIONAL_B_SPLINE_CURVE((1.07140024848292,1.23714644374248,1.07140024848292))
REPRESENTATION_ITEM('')
);
#192=(
BOUNDED_CURVE()
B_SPLINE_CURVE(2,(#7214,#7215,#7216),.UNSPECIFIED.,.F.,.F.)
B_SPLINE_CURVE_WITH_KNOTS((3,3),(0.14973948338295,0.97160236658079),
 .UNSPECIFIED.)
CURVE()
GEOMETRIC_REPRESENTATION_ITEM()
RATIONAL_B_SPLINE_CURVE((1.07140024848292,1.23714644374248,1.07140024848292))
REPRESENTATION_ITEM('')
);
#193=(
BOUNDED_CURVE()
B_SPLINE_CURVE(2,(#7223,#7224,#7225),.UNSPECIFIED.,.F.,.F.)
B_SPLINE_CURVE_WITH_KNOTS((3,3),(0.14973948338295,0.97160236658079),
 .UNSPECIFIED.)
CURVE()
GEOMETRIC_REPRESENTATION_ITEM()
RATIONAL_B_SPLINE_CURVE((1.07140024848292,1.23714644374248,1.07140024848292))
REPRESENTATION_ITEM('')
);
#194=(
BOUNDED_CURVE()
B_SPLINE_CURVE(2,(#7227,#7228,#7229),.UNSPECIFIED.,.F.,.F.)
B_SPLINE_CURVE_WITH_KNOTS((3,3),(0.14973948338295,0.97160236658079),
 .UNSPECIFIED.)
CURVE()
GEOMETRIC_REPRESENTATION_ITEM()
RATIONAL_B_SPLINE_CURVE((1.07140024848292,1.23714644374248,1.07140024848292))
REPRESENTATION_ITEM('')
);
#195=(
BOUNDED_CURVE()
B_SPLINE_CURVE(2,(#7231,#7232,#7233),.UNSPECIFIED.,.F.,.F.)
B_SPLINE_CURVE_WITH_KNOTS((3,3),(0.14973948338295,0.971602366580789),
 .UNSPECIFIED.)
CURVE()
GEOMETRIC_REPRESENTATION_ITEM()
RATIONAL_B_SPLINE_CURVE((1.07140024848292,1.23714644374248,1.07140024848292))
REPRESENTATION_ITEM('')
);
#196=(
BOUNDED_CURVE()
B_SPLINE_CURVE(2,(#7235,#7236,#7237),.UNSPECIFIED.,.F.,.F.)
B_SPLINE_CURVE_WITH_KNOTS((3,3),(0.14973948338295,0.97160236658079),
 .UNSPECIFIED.)
CURVE()
GEOMETRIC_REPRESENTATION_ITEM()
RATIONAL_B_SPLINE_CURVE((1.07140024848292,1.23714644374248,1.07140024848292))
REPRESENTATION_ITEM('')
);
#197=(
BOUNDED_CURVE()
B_SPLINE_CURVE(2,(#7239,#7240,#7241),.UNSPECIFIED.,.F.,.F.)
B_SPLINE_CURVE_WITH_KNOTS((3,3),(0.14973948338295,0.97160236658079),
 .UNSPECIFIED.)
CURVE()
GEOMETRIC_REPRESENTATION_ITEM()
RATIONAL_B_SPLINE_CURVE((1.07140024848292,1.23714644374248,1.07140024848292))
REPRESENTATION_ITEM('')
);
#198=(
BOUNDED_CURVE()
B_SPLINE_CURVE(2,(#7242,#7243,#7244),.UNSPECIFIED.,.F.,.F.)
B_SPLINE_CURVE_WITH_KNOTS((3,3),(0.14973948338295,0.971602366580789),
 .UNSPECIFIED.)
CURVE()
GEOMETRIC_REPRESENTATION_ITEM()
RATIONAL_B_SPLINE_CURVE((1.07140024848292,1.23714644374248,1.07140024848292))
REPRESENTATION_ITEM('')
);
#199=ORIENTED_CLOSED_SHELL('',*,#4158,.F.);
#200=ORIENTED_CLOSED_SHELL('',*,#4160,.F.);
#201=ORIENTED_CLOSED_SHELL('',*,#4167,.F.);
#202=CONICAL_SURFACE('',#4623,0.475,0.785398163397449);
#203=CONICAL_SURFACE('',#4627,0.485,0.785398163397448);
#204=CONICAL_SURFACE('',#4631,0.31,0.463647609000806);
#205=CONICAL_SURFACE('',#4635,0.27,0.785398163397448);
#206=CONICAL_SURFACE('',#4649,0.4,0.785398163397448);
#207=CONICAL_SURFACE('',#4653,0.41,0.785398163397448);
#208=CONICAL_SURFACE('',#4657,0.26,0.463647609000806);
#209=CONICAL_SURFACE('',#4661,0.225,0.785398163397448);
#210=CONICAL_SURFACE('',#4682,0.47094010767585,1.0471975511966);
#211=CONICAL_SURFACE('',#4684,0.47094010767585,1.0471975511966);
#212=CONICAL_SURFACE('',#4782,0.325,0.785398163397448);
#213=CONICAL_SURFACE('',#4786,0.335,0.785398163397448);
#214=CONICAL_SURFACE('',#4790,0.21,0.463647609000806);
#215=CONICAL_SURFACE('',#4803,0.734027674973257,1.0471975511966);
#216=CONICAL_SURFACE('',#4805,0.734027674973257,1.0471975511966);
#217=BREP_WITH_VOIDS('Body1',#4157,(#199));
#218=BREP_WITH_VOIDS('Body1',#4159,(#200));
#219=BREP_WITH_VOIDS('Body1',#4168,(#201));
#220=ELLIPSE('',#4506,0.707106781186547,0.5);
#221=ELLIPSE('',#4518,0.707106781186547,0.5);
#222=ELLIPSE('',#4545,0.707106781186547,0.5);
#223=ELLIPSE('',#4557,0.707106781186547,0.5);
#224=SHAPE_REPRESENTATION_RELATIONSHIP('SRR','None',#7442,#245);
#225=SHAPE_REPRESENTATION_RELATIONSHIP('SRR','None',#7443,#246);
#226=SHAPE_REPRESENTATION_RELATIONSHIP('SRR','None',#7444,#247);
#227=SHAPE_REPRESENTATION_RELATIONSHIP('SRR','None',#7445,#248);
#228=SHAPE_REPRESENTATION_RELATIONSHIP('SRR','None',#7446,#249);
#229=SHAPE_REPRESENTATION_RELATIONSHIP('SRR','None',#7447,#250);
#230=SHAPE_REPRESENTATION_RELATIONSHIP('SRR','None',#7448,#251);
#231=SHAPE_REPRESENTATION_RELATIONSHIP('SRR','None',#7449,#252);
#232=SHAPE_REPRESENTATION_RELATIONSHIP('SRR','None',#7450,#253);
#233=SHAPE_REPRESENTATION_RELATIONSHIP('SRR','None',#7451,#254);
#234=SHAPE_REPRESENTATION_RELATIONSHIP('SRR','None',#7452,#255);
#235=SHAPE_REPRESENTATION_RELATIONSHIP('SRR','None',#7453,#256);
#236=SHAPE_REPRESENTATION_RELATIONSHIP('SRR','None',#7454,#257);
#237=SHAPE_REPRESENTATION_RELATIONSHIP('SRR','None',#7456,#258);
#238=SHAPE_REPRESENTATION_RELATIONSHIP('SRR','None',#7457,#259);
#239=SHAPE_REPRESENTATION_RELATIONSHIP('SRR','None',#7458,#260);
#240=SHAPE_REPRESENTATION_RELATIONSHIP('SRR','None',#7459,#261);
#241=SHAPE_REPRESENTATION_RELATIONSHIP('SRR','None',#7460,#262);
#242=SHAPE_REPRESENTATION_RELATIONSHIP('SRR','None',#7461,#263);
#243=SHAPE_REPRESENTATION_RELATIONSHIP('SRR','None',#7462,#264);
#244=SHAPE_REPRESENTATION_RELATIONSHIP('SRR','None',#7464,#265);
#245=ADVANCED_BREP_SHAPE_REPRESENTATION('',(#287),#7321);
#246=ADVANCED_BREP_SHAPE_REPRESENTATION('',(#288),#7322);
#247=ADVANCED_BREP_SHAPE_REPRESENTATION('',(#289),#7323);
#248=ADVANCED_BREP_SHAPE_REPRESENTATION('',(#290),#7324);
#249=ADVANCED_BREP_SHAPE_REPRESENTATION('',(#291),#7325);
#250=ADVANCED_BREP_SHAPE_REPRESENTATION('',(#292),#7326);
#251=ADVANCED_BREP_SHAPE_REPRESENTATION('',(#293),#7327);
#252=ADVANCED_BREP_SHAPE_REPRESENTATION('',(#294),#7328);
#253=ADVANCED_BREP_SHAPE_REPRESENTATION('',(#295),#7329);
#254=ADVANCED_BREP_SHAPE_REPRESENTATION('',(#217),#7330);
#255=ADVANCED_BREP_SHAPE_REPRESENTATION('',(#218),#7331);
#256=ADVANCED_BREP_SHAPE_REPRESENTATION('',(#296),#7332);
#257=ADVANCED_BREP_SHAPE_REPRESENTATION('',(#297),#7333);
#258=ADVANCED_BREP_SHAPE_REPRESENTATION('',(#298),#7335);
#259=ADVANCED_BREP_SHAPE_REPRESENTATION('',(#299),#7336);
#260=ADVANCED_BREP_SHAPE_REPRESENTATION('',(#300),#7337);
#261=ADVANCED_BREP_SHAPE_REPRESENTATION('',(#301),#7338);
#262=ADVANCED_BREP_SHAPE_REPRESENTATION('',(#219),#7339);
#263=ADVANCED_BREP_SHAPE_REPRESENTATION('',(#302),#7340);
#264=ADVANCED_BREP_SHAPE_REPRESENTATION('',(#303),#7341);
#265=ADVANCED_BREP_SHAPE_REPRESENTATION('',(#304),#7343);
#266=STYLED_ITEM('',(#7610),#287);
#267=STYLED_ITEM('',(#7645),#288);
#268=STYLED_ITEM('',(#7624),#289);
#269=STYLED_ITEM('',(#7645),#290);
#270=STYLED_ITEM('',(#7624),#291);
#271=STYLED_ITEM('',(#7610),#292);
#272=STYLED_ITEM('',(#7610),#293);
#273=STYLED_ITEM('',(#7624),#294);
#274=STYLED_ITEM('',(#7631),#295);
#275=STYLED_ITEM('',(#7638),#217);
#276=STYLED_ITEM('',(#7638),#218);
#277=STYLED_ITEM('',(#7638),#296);
#278=STYLED_ITEM('',(#7638),#297);
#279=STYLED_ITEM('',(#7645),#298);
#280=STYLED_ITEM('',(#7624),#299);
#281=STYLED_ITEM('',(#7638),#300);
#282=STYLED_ITEM('',(#7638),#301);
#283=STYLED_ITEM('',(#7638),#219);
#284=STYLED_ITEM('',(#7638),#302);
#285=STYLED_ITEM('',(#7638),#303);
#286=STYLED_ITEM('',(#7624),#304);
#287=MANIFOLD_SOLID_BREP('Body1',#4148);
#288=MANIFOLD_SOLID_BREP('Body1',#4149);
#289=MANIFOLD_SOLID_BREP('Body1',#4150);
#290=MANIFOLD_SOLID_BREP('Body1',#4151);
#291=MANIFOLD_SOLID_BREP('Body1',#4152);
#292=MANIFOLD_SOLID_BREP('Body1',#4153);
#293=MANIFOLD_SOLID_BREP('Body1',#4154);
#294=MANIFOLD_SOLID_BREP('Body1',#4155);
#295=MANIFOLD_SOLID_BREP('Body1',#4156);
#296=MANIFOLD_SOLID_BREP('Body1',#4161);
#297=MANIFOLD_SOLID_BREP('Body1',#4162);
#298=MANIFOLD_SOLID_BREP('Body1',#4163);
#299=MANIFOLD_SOLID_BREP('Body1',#4164);
#300=MANIFOLD_SOLID_BREP('Body1',#4165);
#301=MANIFOLD_SOLID_BREP('Body1',#4166);
#302=MANIFOLD_SOLID_BREP('Body1',#4169);
#303=MANIFOLD_SOLID_BREP('Body1',#4170);
#304=MANIFOLD_SOLID_BREP('Body1',#4171);
#305=FACE_BOUND('',#829,.T.);
#306=FACE_BOUND('',#830,.T.);
#307=FACE_BOUND('',#831,.T.);
#308=FACE_BOUND('',#832,.T.);
#309=FACE_BOUND('',#833,.T.);
#310=FACE_BOUND('',#834,.T.);
#311=FACE_BOUND('',#835,.T.);
#312=FACE_BOUND('',#836,.T.);
#313=FACE_BOUND('',#837,.T.);
#314=FACE_BOUND('',#838,.T.);
#315=FACE_BOUND('',#839,.T.);
#316=FACE_BOUND('',#840,.T.);
#317=FACE_BOUND('',#841,.T.);
#318=FACE_BOUND('',#842,.T.);
#319=FACE_BOUND('',#844,.T.);
#320=FACE_BOUND('',#845,.T.);
#321=FACE_BOUND('',#846,.T.);
#322=FACE_BOUND('',#847,.T.);
#323=FACE_BOUND('',#848,.T.);
#324=FACE_BOUND('',#849,.T.);
#325=FACE_BOUND('',#850,.T.);
#326=FACE_BOUND('',#851,.T.);
#327=FACE_BOUND('',#852,.T.);
#328=FACE_BOUND('',#853,.T.);
#329=FACE_BOUND('',#854,.T.);
#330=FACE_BOUND('',#855,.T.);
#331=FACE_BOUND('',#863,.T.);
#332=FACE_BOUND('',#864,.T.);
#333=FACE_BOUND('',#866,.T.);
#334=FACE_BOUND('',#867,.T.);
#335=FACE_BOUND('',#881,.T.);
#336=FACE_BOUND('',#882,.T.);
#337=FACE_BOUND('',#884,.T.);
#338=FACE_BOUND('',#885,.T.);
#339=FACE_BOUND('',#901,.T.);
#340=FACE_BOUND('',#904,.T.);
#341=FACE_BOUND('',#918,.T.);
#342=FACE_BOUND('',#919,.T.);
#343=FACE_BOUND('',#920,.T.);
#344=FACE_BOUND('',#930,.T.);
#345=FACE_BOUND('',#933,.T.);
#346=FACE_BOUND('',#947,.T.);
#347=FACE_BOUND('',#948,.T.);
#348=FACE_BOUND('',#949,.T.);
#349=FACE_BOUND('',#954,.T.);
#350=FACE_BOUND('',#958,.T.);
#351=FACE_BOUND('',#966,.T.);
#352=FACE_BOUND('',#969,.T.);
#353=FACE_BOUND('',#971,.T.);
#354=FACE_BOUND('',#972,.T.);
#355=FACE_BOUND('',#988,.T.);
#356=FACE_BOUND('',#1006,.T.);
#357=FACE_BOUND('',#1022,.T.);
#358=FACE_BOUND('',#1024,.T.);
#359=FACE_BOUND('',#1035,.T.);
#360=FACE_BOUND('',#1037,.T.);
#361=FACE_BOUND('',#1047,.T.);
#362=FACE_BOUND('',#1048,.T.);
#363=FACE_BOUND('',#1049,.T.);
#364=FACE_BOUND('',#1050,.T.);
#365=FACE_BOUND('',#1052,.T.);
#366=FACE_BOUND('',#1053,.T.);
#367=FACE_BOUND('',#1054,.T.);
#368=FACE_BOUND('',#1055,.T.);
#369=FACE_BOUND('',#1066,.T.);
#370=FACE_BOUND('',#1067,.T.);
#371=FACE_BOUND('',#1088,.T.);
#372=FACE_BOUND('',#1094,.T.);
#373=FACE_BOUND('',#1096,.T.);
#374=FACE_BOUND('',#1107,.T.);
#375=FACE_BOUND('',#1109,.T.);
#376=CIRCLE('',#4418,0.274999999999999);
#377=CIRCLE('',#4419,0.274999999999999);
#378=CIRCLE('',#4421,0.275);
#379=CIRCLE('',#4422,0.275);
#380=CIRCLE('',#4424,0.275);
#381=CIRCLE('',#4425,0.275);
#382=CIRCLE('',#4427,0.274999999999999);
#383=CIRCLE('',#4428,0.274999999999999);
#384=CIRCLE('',#4430,0.34);
#385=CIRCLE('',#4431,0.34);
#386=CIRCLE('',#4433,0.34);
#387=CIRCLE('',#4434,0.34);
#388=CIRCLE('',#4436,0.25);
#389=CIRCLE('',#4437,0.25);
#390=CIRCLE('',#4439,0.25);
#391=CIRCLE('',#4440,0.25);
#392=CIRCLE('',#4442,0.25);
#393=CIRCLE('',#4443,0.25);
#394=CIRCLE('',#4445,0.25);
#395=CIRCLE('',#4446,0.25);
#396=CIRCLE('',#4448,0.25);
#397=CIRCLE('',#4449,0.25);
#398=CIRCLE('',#4451,0.25);
#399=CIRCLE('',#4452,0.25);
#400=CIRCLE('',#4461,0.21);
#401=CIRCLE('',#4462,0.21);
#402=CIRCLE('',#4464,0.21);
#403=CIRCLE('',#4465,0.21);
#404=CIRCLE('',#4481,0.210000000000001);
#405=CIRCLE('',#4482,0.210000000000001);
#406=CIRCLE('',#4484,0.210000000000001);
#407=CIRCLE('',#4485,0.210000000000001);
#408=CIRCLE('',#4501,0.5);
#409=CIRCLE('',#4502,0.5);
#410=CIRCLE('',#4504,0.5);
#411=CIRCLE('',#4505,0.5);
#412=CIRCLE('',#4513,0.5);
#413=CIRCLE('',#4514,0.5);
#414=CIRCLE('',#4516,0.33);
#415=CIRCLE('',#4519,0.5);
#416=CIRCLE('',#4520,0.5);
#417=CIRCLE('',#4522,0.33);
#418=CIRCLE('',#4528,0.33);
#419=CIRCLE('',#4530,0.33);
#420=CIRCLE('',#4540,0.5);
#421=CIRCLE('',#4541,0.5);
#422=CIRCLE('',#4543,0.5);
#423=CIRCLE('',#4544,0.5);
#424=CIRCLE('',#4552,0.5);
#425=CIRCLE('',#4553,0.5);
#426=CIRCLE('',#4555,0.33);
#427=CIRCLE('',#4558,0.5);
#428=CIRCLE('',#4559,0.5);
#429=CIRCLE('',#4561,0.33);
#430=CIRCLE('',#4567,0.33);
#431=CIRCLE('',#4569,0.33);
#432=CIRCLE('',#4579,0.21);
#433=CIRCLE('',#4580,0.21);
#434=CIRCLE('',#4582,0.5);
#435=CIRCLE('',#4583,0.5);
#436=CIRCLE('',#4585,0.5);
#437=CIRCLE('',#4586,0.5);
#438=CIRCLE('',#4588,0.33);
#439=CIRCLE('',#4590,0.5);
#440=CIRCLE('',#4591,0.5);
#441=CIRCLE('',#4593,0.5);
#442=CIRCLE('',#4594,0.5);
#443=CIRCLE('',#4596,0.33);
#444=CIRCLE('',#4601,0.33);
#445=CIRCLE('',#4603,0.33);
#446=CIRCLE('',#4622,0.45);
#447=CIRCLE('',#4624,0.5);
#448=CIRCLE('',#4626,0.5);
#449=CIRCLE('',#4628,0.47);
#450=CIRCLE('',#4630,0.32);
#451=CIRCLE('',#4632,0.2942);
#452=CIRCLE('',#4634,0.2942);
#453=CIRCLE('',#4636,0.24);
#454=CIRCLE('',#4648,0.375);
#455=CIRCLE('',#4650,0.425);
#456=CIRCLE('',#4652,0.425);
#457=CIRCLE('',#4654,0.395);
#458=CIRCLE('',#4656,0.27);
#459=CIRCLE('',#4658,0.24505);
#460=CIRCLE('',#4660,0.24505);
#461=CIRCLE('',#4662,0.2);
#462=CIRCLE('',#4674,0.265);
#463=CIRCLE('',#4675,0.265);
#464=CIRCLE('',#4677,0.5);
#465=CIRCLE('',#4678,0.5);
#466=CIRCLE('',#4683,0.38);
#467=CIRCLE('',#4685,0.38);
#468=CIRCLE('',#4690,0.2117);
#469=CIRCLE('',#4691,0.2117);
#470=CIRCLE('',#4723,0.225);
#471=CIRCLE('',#4724,0.225);
#472=CIRCLE('',#4726,0.225);
#473=CIRCLE('',#4727,0.225);
#474=CIRCLE('',#4729,0.449999999999999);
#475=CIRCLE('',#4730,0.449999999999999);
#476=CIRCLE('',#4732,0.449999999999999);
#477=CIRCLE('',#4733,0.449999999999999);
#478=CIRCLE('',#4742,0.164999999999999);
#479=CIRCLE('',#4743,0.164999999999999);
#480=CIRCLE('',#4746,0.164999999999999);
#481=CIRCLE('',#4747,0.164999999999999);
#482=CIRCLE('',#4750,1.5);
#483=CIRCLE('',#4751,1.5);
#484=CIRCLE('',#4759,0.3933);
#485=CIRCLE('',#4760,0.3933);
#486=CIRCLE('',#4765,0.3933);
#487=CIRCLE('',#4766,0.3933);
#488=CIRCLE('',#4779,0.1954);
#489=CIRCLE('',#4781,0.3);
#490=CIRCLE('',#4783,0.35);
#491=CIRCLE('',#4785,0.35);
#492=CIRCLE('',#4787,0.32);
#493=CIRCLE('',#4789,0.22);
#494=CIRCLE('',#4791,0.1954);
#495=CIRCLE('',#4795,0.42);
#496=CIRCLE('',#4796,0.42);
#497=CIRCLE('',#4798,0.8);
#498=CIRCLE('',#4799,0.8);
#499=CIRCLE('',#4804,0.6175);
#500=CIRCLE('',#4806,0.6175);
#501=CIRCLE('',#4811,0.338975);
#502=CIRCLE('',#4812,0.338975);
#503=CIRCLE('',#4835,1.5);
#504=CIRCLE('',#4836,1.5);
#505=CYLINDRICAL_SURFACE('',#4417,0.274999999999999);
#506=CYLINDRICAL_SURFACE('',#4420,0.275);
#507=CYLINDRICAL_SURFACE('',#4423,0.275);
#508=CYLINDRICAL_SURFACE('',#4426,0.274999999999999);
#509=CYLINDRICAL_SURFACE('',#4429,0.34);
#510=CYLINDRICAL_SURFACE('',#4432,0.34);
#511=CYLINDRICAL_SURFACE('',#4435,0.25);
#512=CYLINDRICAL_SURFACE('',#4438,0.25);
#513=CYLINDRICAL_SURFACE('',#4441,0.25);
#514=CYLINDRICAL_SURFACE('',#4444,0.25);
#515=CYLINDRICAL_SURFACE('',#4447,0.25);
#516=CYLINDRICAL_SURFACE('',#4450,0.25);
#517=CYLINDRICAL_SURFACE('',#4460,0.21);
#518=CYLINDRICAL_SURFACE('',#4463,0.21);
#519=CYLINDRICAL_SURFACE('',#4480,0.210000000000001);
#520=CYLINDRICAL_SURFACE('',#4483,0.210000000000001);
#521=CYLINDRICAL_SURFACE('',#4500,0.5);
#522=CYLINDRICAL_SURFACE('',#4503,0.5);
#523=CYLINDRICAL_SURFACE('',#4512,0.5);
#524=CYLINDRICAL_SURFACE('',#4517,0.5);
#525=CYLINDRICAL_SURFACE('',#4527,0.33);
#526=CYLINDRICAL_SURFACE('',#4529,0.33);
#527=CYLINDRICAL_SURFACE('',#4539,0.5);
#528=CYLINDRICAL_SURFACE('',#4542,0.5);
#529=CYLINDRICAL_SURFACE('',#4551,0.5);
#530=CYLINDRICAL_SURFACE('',#4556,0.5);
#531=CYLINDRICAL_SURFACE('',#4566,0.33);
#532=CYLINDRICAL_SURFACE('',#4568,0.33);
#533=CYLINDRICAL_SURFACE('',#4578,0.21);
#534=CYLINDRICAL_SURFACE('',#4581,0.5);
#535=CYLINDRICAL_SURFACE('',#4584,0.5);
#536=CYLINDRICAL_SURFACE('',#4589,0.5);
#537=CYLINDRICAL_SURFACE('',#4592,0.5);
#538=CYLINDRICAL_SURFACE('',#4600,0.33);
#539=CYLINDRICAL_SURFACE('',#4602,0.33);
#540=CYLINDRICAL_SURFACE('',#4625,0.5);
#541=CYLINDRICAL_SURFACE('',#4633,0.2942);
#542=CYLINDRICAL_SURFACE('',#4651,0.425);
#543=CYLINDRICAL_SURFACE('',#4659,0.24505);
#544=CYLINDRICAL_SURFACE('',#4673,0.265);
#545=CYLINDRICAL_SURFACE('',#4676,0.5);
#546=CYLINDRICAL_SURFACE('',#4689,0.2117);
#547=CYLINDRICAL_SURFACE('',#4722,0.225);
#548=CYLINDRICAL_SURFACE('',#4725,0.225);
#549=CYLINDRICAL_SURFACE('',#4728,0.449999999999999);
#550=CYLINDRICAL_SURFACE('',#4731,0.449999999999999);
#551=CYLINDRICAL_SURFACE('',#4741,0.164999999999999);
#552=CYLINDRICAL_SURFACE('',#4745,0.164999999999999);
#553=CYLINDRICAL_SURFACE('',#4749,1.5);
#554=CYLINDRICAL_SURFACE('',#4758,0.3933);
#555=CYLINDRICAL_SURFACE('',#4764,0.3933);
#556=CYLINDRICAL_SURFACE('',#4784,0.35);
#557=CYLINDRICAL_SURFACE('',#4792,0.1954);
#558=CYLINDRICAL_SURFACE('',#4794,0.42);
#559=CYLINDRICAL_SURFACE('',#4797,0.8);
#560=CYLINDRICAL_SURFACE('',#4810,0.338975);
#561=CYLINDRICAL_SURFACE('',#4834,1.5);
#562=FACE_OUTER_BOUND('',#802,.T.);
#563=FACE_OUTER_BOUND('',#803,.T.);
#564=FACE_OUTER_BOUND('',#804,.T.);
#565=FACE_OUTER_BOUND('',#805,.T.);
#566=FACE_OUTER_BOUND('',#806,.T.);
#567=FACE_OUTER_BOUND('',#807,.T.);
#568=FACE_OUTER_BOUND('',#808,.T.);
#569=FACE_OUTER_BOUND('',#809,.T.);
#570=FACE_OUTER_BOUND('',#810,.T.);
#571=FACE_OUTER_BOUND('',#811,.T.);
#572=FACE_OUTER_BOUND('',#812,.T.);
#573=FACE_OUTER_BOUND('',#813,.T.);
#574=FACE_OUTER_BOUND('',#814,.T.);
#575=FACE_OUTER_BOUND('',#815,.T.);
#576=FACE_OUTER_BOUND('',#816,.T.);
#577=FACE_OUTER_BOUND('',#817,.T.);
#578=FACE_OUTER_BOUND('',#818,.T.);
#579=FACE_OUTER_BOUND('',#819,.T.);
#580=FACE_OUTER_BOUND('',#820,.T.);
#581=FACE_OUTER_BOUND('',#821,.T.);
#582=FACE_OUTER_BOUND('',#822,.T.);
#583=FACE_OUTER_BOUND('',#823,.T.);
#584=FACE_OUTER_BOUND('',#824,.T.);
#585=FACE_OUTER_BOUND('',#825,.T.);
#586=FACE_OUTER_BOUND('',#826,.T.);
#587=FACE_OUTER_BOUND('',#827,.T.);
#588=FACE_OUTER_BOUND('',#828,.T.);
#589=FACE_OUTER_BOUND('',#843,.T.);
#590=FACE_OUTER_BOUND('',#856,.T.);
#591=FACE_OUTER_BOUND('',#857,.T.);
#592=FACE_OUTER_BOUND('',#858,.T.);
#593=FACE_OUTER_BOUND('',#859,.T.);
#594=FACE_OUTER_BOUND('',#860,.T.);
#595=FACE_OUTER_BOUND('',#861,.T.);
#596=FACE_OUTER_BOUND('',#862,.T.);
#597=FACE_OUTER_BOUND('',#865,.T.);
#598=FACE_OUTER_BOUND('',#868,.T.);
#599=FACE_OUTER_BOUND('',#869,.T.);
#600=FACE_OUTER_BOUND('',#870,.T.);
#601=FACE_OUTER_BOUND('',#871,.T.);
#602=FACE_OUTER_BOUND('',#872,.T.);
#603=FACE_OUTER_BOUND('',#873,.T.);
#604=FACE_OUTER_BOUND('',#874,.T.);
#605=FACE_OUTER_BOUND('',#875,.T.);
#606=FACE_OUTER_BOUND('',#876,.T.);
#607=FACE_OUTER_BOUND('',#877,.T.);
#608=FACE_OUTER_BOUND('',#878,.T.);
#609=FACE_OUTER_BOUND('',#879,.T.);
#610=FACE_OUTER_BOUND('',#880,.T.);
#611=FACE_OUTER_BOUND('',#883,.T.);
#612=FACE_OUTER_BOUND('',#886,.T.);
#613=FACE_OUTER_BOUND('',#887,.T.);
#614=FACE_OUTER_BOUND('',#888,.T.);
#615=FACE_OUTER_BOUND('',#889,.T.);
#616=FACE_OUTER_BOUND('',#890,.T.);
#617=FACE_OUTER_BOUND('',#891,.T.);
#618=FACE_OUTER_BOUND('',#892,.T.);
#619=FACE_OUTER_BOUND('',#893,.T.);
#620=FACE_OUTER_BOUND('',#894,.T.);
#621=FACE_OUTER_BOUND('',#895,.T.);
#622=FACE_OUTER_BOUND('',#896,.T.);
#623=FACE_OUTER_BOUND('',#897,.T.);
#624=FACE_OUTER_BOUND('',#898,.T.);
#625=FACE_OUTER_BOUND('',#899,.T.);
#626=FACE_OUTER_BOUND('',#900,.T.);
#627=FACE_OUTER_BOUND('',#902,.T.);
#628=FACE_OUTER_BOUND('',#903,.T.);
#629=FACE_OUTER_BOUND('',#905,.T.);
#630=FACE_OUTER_BOUND('',#906,.T.);
#631=FACE_OUTER_BOUND('',#907,.T.);
#632=FACE_OUTER_BOUND('',#908,.T.);
#633=FACE_OUTER_BOUND('',#909,.T.);
#634=FACE_OUTER_BOUND('',#910,.T.);
#635=FACE_OUTER_BOUND('',#911,.T.);
#636=FACE_OUTER_BOUND('',#912,.T.);
#637=FACE_OUTER_BOUND('',#913,.T.);
#638=FACE_OUTER_BOUND('',#914,.T.);
#639=FACE_OUTER_BOUND('',#915,.T.);
#640=FACE_OUTER_BOUND('',#916,.T.);
#641=FACE_OUTER_BOUND('',#917,.T.);
#642=FACE_OUTER_BOUND('',#921,.T.);
#643=FACE_OUTER_BOUND('',#922,.T.);
#644=FACE_OUTER_BOUND('',#923,.T.);
#645=FACE_OUTER_BOUND('',#924,.T.);
#646=FACE_OUTER_BOUND('',#925,.T.);
#647=FACE_OUTER_BOUND('',#926,.T.);
#648=FACE_OUTER_BOUND('',#927,.T.);
#649=FACE_OUTER_BOUND('',#928,.T.);
#650=FACE_OUTER_BOUND('',#929,.T.);
#651=FACE_OUTER_BOUND('',#931,.T.);
#652=FACE_OUTER_BOUND('',#932,.T.);
#653=FACE_OUTER_BOUND('',#934,.T.);
#654=FACE_OUTER_BOUND('',#935,.T.);
#655=FACE_OUTER_BOUND('',#936,.T.);
#656=FACE_OUTER_BOUND('',#937,.T.);
#657=FACE_OUTER_BOUND('',#938,.T.);
#658=FACE_OUTER_BOUND('',#939,.T.);
#659=FACE_OUTER_BOUND('',#940,.T.);
#660=FACE_OUTER_BOUND('',#941,.T.);
#661=FACE_OUTER_BOUND('',#942,.T.);
#662=FACE_OUTER_BOUND('',#943,.T.);
#663=FACE_OUTER_BOUND('',#944,.T.);
#664=FACE_OUTER_BOUND('',#945,.T.);
#665=FACE_OUTER_BOUND('',#946,.T.);
#666=FACE_OUTER_BOUND('',#950,.T.);
#667=FACE_OUTER_BOUND('',#951,.T.);
#668=FACE_OUTER_BOUND('',#952,.T.);
#669=FACE_OUTER_BOUND('',#953,.T.);
#670=FACE_OUTER_BOUND('',#955,.T.);
#671=FACE_OUTER_BOUND('',#956,.T.);
#672=FACE_OUTER_BOUND('',#957,.T.);
#673=FACE_OUTER_BOUND('',#959,.T.);
#674=FACE_OUTER_BOUND('',#960,.T.);
#675=FACE_OUTER_BOUND('',#961,.T.);
#676=FACE_OUTER_BOUND('',#962,.T.);
#677=FACE_OUTER_BOUND('',#963,.T.);
#678=FACE_OUTER_BOUND('',#964,.T.);
#679=FACE_OUTER_BOUND('',#965,.T.);
#680=FACE_OUTER_BOUND('',#967,.T.);
#681=FACE_OUTER_BOUND('',#968,.T.);
#682=FACE_OUTER_BOUND('',#970,.T.);
#683=FACE_OUTER_BOUND('',#973,.T.);
#684=FACE_OUTER_BOUND('',#974,.T.);
#685=FACE_OUTER_BOUND('',#975,.T.);
#686=FACE_OUTER_BOUND('',#976,.T.);
#687=FACE_OUTER_BOUND('',#977,.T.);
#688=FACE_OUTER_BOUND('',#978,.T.);
#689=FACE_OUTER_BOUND('',#979,.T.);
#690=FACE_OUTER_BOUND('',#980,.T.);
#691=FACE_OUTER_BOUND('',#981,.T.);
#692=FACE_OUTER_BOUND('',#982,.T.);
#693=FACE_OUTER_BOUND('',#983,.T.);
#694=FACE_OUTER_BOUND('',#984,.T.);
#695=FACE_OUTER_BOUND('',#985,.T.);
#696=FACE_OUTER_BOUND('',#986,.T.);
#697=FACE_OUTER_BOUND('',#987,.T.);
#698=FACE_OUTER_BOUND('',#989,.T.);
#699=FACE_OUTER_BOUND('',#990,.T.);
#700=FACE_OUTER_BOUND('',#991,.T.);
#701=FACE_OUTER_BOUND('',#992,.T.);
#702=FACE_OUTER_BOUND('',#993,.T.);
#703=FACE_OUTER_BOUND('',#994,.T.);
#704=FACE_OUTER_BOUND('',#995,.T.);
#705=FACE_OUTER_BOUND('',#996,.T.);
#706=FACE_OUTER_BOUND('',#997,.T.);
#707=FACE_OUTER_BOUND('',#998,.T.);
#708=FACE_OUTER_BOUND('',#999,.T.);
#709=FACE_OUTER_BOUND('',#1000,.T.);
#710=FACE_OUTER_BOUND('',#1001,.T.);
#711=FACE_OUTER_BOUND('',#1002,.T.);
#712=FACE_OUTER_BOUND('',#1003,.T.);
#713=FACE_OUTER_BOUND('',#1004,.T.);
#714=FACE_OUTER_BOUND('',#1005,.T.);
#715=FACE_OUTER_BOUND('',#1007,.T.);
#716=FACE_OUTER_BOUND('',#1008,.T.);
#717=FACE_OUTER_BOUND('',#1009,.T.);
#718=FACE_OUTER_BOUND('',#1010,.T.);
#719=FACE_OUTER_BOUND('',#1011,.T.);
#720=FACE_OUTER_BOUND('',#1012,.T.);
#721=FACE_OUTER_BOUND('',#1013,.T.);
#722=FACE_OUTER_BOUND('',#1014,.T.);
#723=FACE_OUTER_BOUND('',#1015,.T.);
#724=FACE_OUTER_BOUND('',#1016,.T.);
#725=FACE_OUTER_BOUND('',#1017,.T.);
#726=FACE_OUTER_BOUND('',#1018,.T.);
#727=FACE_OUTER_BOUND('',#1019,.T.);
#728=FACE_OUTER_BOUND('',#1020,.T.);
#729=FACE_OUTER_BOUND('',#1021,.T.);
#730=FACE_OUTER_BOUND('',#1023,.T.);
#731=FACE_OUTER_BOUND('',#1025,.T.);
#732=FACE_OUTER_BOUND('',#1026,.T.);
#733=FACE_OUTER_BOUND('',#1027,.T.);
#734=FACE_OUTER_BOUND('',#1028,.T.);
#735=FACE_OUTER_BOUND('',#1029,.T.);
#736=FACE_OUTER_BOUND('',#1030,.T.);
#737=FACE_OUTER_BOUND('',#1031,.T.);
#738=FACE_OUTER_BOUND('',#1032,.T.);
#739=FACE_OUTER_BOUND('',#1033,.T.);
#740=FACE_OUTER_BOUND('',#1034,.T.);
#741=FACE_OUTER_BOUND('',#1036,.T.);
#742=FACE_OUTER_BOUND('',#1038,.T.);
#743=FACE_OUTER_BOUND('',#1039,.T.);
#744=FACE_OUTER_BOUND('',#1040,.T.);
#745=FACE_OUTER_BOUND('',#1041,.T.);
#746=FACE_OUTER_BOUND('',#1042,.T.);
#747=FACE_OUTER_BOUND('',#1043,.T.);
#748=FACE_OUTER_BOUND('',#1044,.T.);
#749=FACE_OUTER_BOUND('',#1045,.T.);
#750=FACE_OUTER_BOUND('',#1046,.T.);
#751=FACE_OUTER_BOUND('',#1051,.T.);
#752=FACE_OUTER_BOUND('',#1056,.T.);
#753=FACE_OUTER_BOUND('',#1057,.T.);
#754=FACE_OUTER_BOUND('',#1058,.T.);
#755=FACE_OUTER_BOUND('',#1059,.T.);
#756=FACE_OUTER_BOUND('',#1060,.T.);
#757=FACE_OUTER_BOUND('',#1061,.T.);
#758=FACE_OUTER_BOUND('',#1062,.T.);
#759=FACE_OUTER_BOUND('',#1063,.T.);
#760=FACE_OUTER_BOUND('',#1064,.T.);
#761=FACE_OUTER_BOUND('',#1065,.T.);
#762=FACE_OUTER_BOUND('',#1068,.T.);
#763=FACE_OUTER_BOUND('',#1069,.T.);
#764=FACE_OUTER_BOUND('',#1070,.T.);
#765=FACE_OUTER_BOUND('',#1071,.T.);
#766=FACE_OUTER_BOUND('',#1072,.T.);
#767=FACE_OUTER_BOUND('',#1073,.T.);
#768=FACE_OUTER_BOUND('',#1074,.T.);
#769=FACE_OUTER_BOUND('',#1075,.T.);
#770=FACE_OUTER_BOUND('',#1076,.T.);
#771=FACE_OUTER_BOUND('',#1077,.T.);
#772=FACE_OUTER_BOUND('',#1078,.T.);
#773=FACE_OUTER_BOUND('',#1079,.T.);
#774=FACE_OUTER_BOUND('',#1080,.T.);
#775=FACE_OUTER_BOUND('',#1081,.T.);
#776=FACE_OUTER_BOUND('',#1082,.T.);
#777=FACE_OUTER_BOUND('',#1083,.T.);
#778=FACE_OUTER_BOUND('',#1084,.T.);
#779=FACE_OUTER_BOUND('',#1085,.T.);
#780=FACE_OUTER_BOUND('',#1086,.T.);
#781=FACE_OUTER_BOUND('',#1087,.T.);
#782=FACE_OUTER_BOUND('',#1089,.T.);
#783=FACE_OUTER_BOUND('',#1090,.T.);
#784=FACE_OUTER_BOUND('',#1091,.T.);
#785=FACE_OUTER_BOUND('',#1092,.T.);
#786=FACE_OUTER_BOUND('',#1093,.T.);
#787=FACE_OUTER_BOUND('',#1095,.T.);
#788=FACE_OUTER_BOUND('',#1097,.T.);
#789=FACE_OUTER_BOUND('',#1098,.T.);
#790=FACE_OUTER_BOUND('',#1099,.T.);
#791=FACE_OUTER_BOUND('',#1100,.T.);
#792=FACE_OUTER_BOUND('',#1101,.T.);
#793=FACE_OUTER_BOUND('',#1102,.T.);
#794=FACE_OUTER_BOUND('',#1103,.T.);
#795=FACE_OUTER_BOUND('',#1104,.T.);
#796=FACE_OUTER_BOUND('',#1105,.T.);
#797=FACE_OUTER_BOUND('',#1106,.T.);
#798=FACE_OUTER_BOUND('',#1108,.T.);
#799=FACE_OUTER_BOUND('',#1110,.T.);
#800=FACE_OUTER_BOUND('',#1111,.T.);
#801=FACE_OUTER_BOUND('',#1112,.T.);
#802=EDGE_LOOP('',(#2696,#2697,#2698,#2699));
#803=EDGE_LOOP('',(#2700,#2701,#2702,#2703));
#804=EDGE_LOOP('',(#2704,#2705,#2706,#2707));
#805=EDGE_LOOP('',(#2708,#2709,#2710,#2711));
#806=EDGE_LOOP('',(#2712,#2713,#2714,#2715));
#807=EDGE_LOOP('',(#2716,#2717,#2718,#2719));
#808=EDGE_LOOP('',(#2720,#2721,#2722,#2723));
#809=EDGE_LOOP('',(#2724,#2725,#2726,#2727));
#810=EDGE_LOOP('',(#2728,#2729,#2730,#2731));
#811=EDGE_LOOP('',(#2732,#2733,#2734,#2735));
#812=EDGE_LOOP('',(#2736,#2737,#2738,#2739));
#813=EDGE_LOOP('',(#2740,#2741,#2742,#2743));
#814=EDGE_LOOP('',(#2744,#2745,#2746,#2747));
#815=EDGE_LOOP('',(#2748,#2749,#2750,#2751));
#816=EDGE_LOOP('',(#2752,#2753,#2754,#2755));
#817=EDGE_LOOP('',(#2756,#2757,#2758,#2759));
#818=EDGE_LOOP('',(#2760,#2761,#2762,#2763));
#819=EDGE_LOOP('',(#2764,#2765,#2766,#2767));
#820=EDGE_LOOP('',(#2768,#2769,#2770,#2771));
#821=EDGE_LOOP('',(#2772,#2773,#2774,#2775));
#822=EDGE_LOOP('',(#2776,#2777,#2778,#2779));
#823=EDGE_LOOP('',(#2780,#2781,#2782,#2783));
#824=EDGE_LOOP('',(#2784,#2785,#2786,#2787));
#825=EDGE_LOOP('',(#2788,#2789,#2790,#2791));
#826=EDGE_LOOP('',(#2792,#2793,#2794,#2795));
#827=EDGE_LOOP('',(#2796,#2797,#2798,#2799));
#828=EDGE_LOOP('',(#2800,#2801,#2802,#2803));
#829=EDGE_LOOP('',(#2804,#2805,#2806,#2807));
#830=EDGE_LOOP('',(#2808));
#831=EDGE_LOOP('',(#2809));
#832=EDGE_LOOP('',(#2810));
#833=EDGE_LOOP('',(#2811));
#834=EDGE_LOOP('',(#2812));
#835=EDGE_LOOP('',(#2813));
#836=EDGE_LOOP('',(#2814));
#837=EDGE_LOOP('',(#2815));
#838=EDGE_LOOP('',(#2816));
#839=EDGE_LOOP('',(#2817));
#840=EDGE_LOOP('',(#2818));
#841=EDGE_LOOP('',(#2819));
#842=EDGE_LOOP('',(#2820,#2821,#2822,#2823));
#843=EDGE_LOOP('',(#2824,#2825,#2826,#2827));
#844=EDGE_LOOP('',(#2828));
#845=EDGE_LOOP('',(#2829));
#846=EDGE_LOOP('',(#2830));
#847=EDGE_LOOP('',(#2831));
#848=EDGE_LOOP('',(#2832));
#849=EDGE_LOOP('',(#2833));
#850=EDGE_LOOP('',(#2834));
#851=EDGE_LOOP('',(#2835));
#852=EDGE_LOOP('',(#2836));
#853=EDGE_LOOP('',(#2837));
#854=EDGE_LOOP('',(#2838));
#855=EDGE_LOOP('',(#2839));
#856=EDGE_LOOP('',(#2840,#2841,#2842,#2843));
#857=EDGE_LOOP('',(#2844,#2845,#2846,#2847));
#858=EDGE_LOOP('',(#2848,#2849,#2850,#2851));
#859=EDGE_LOOP('',(#2852,#2853,#2854,#2855));
#860=EDGE_LOOP('',(#2856,#2857,#2858,#2859));
#861=EDGE_LOOP('',(#2860,#2861,#2862,#2863));
#862=EDGE_LOOP('',(#2864,#2865,#2866,#2867));
#863=EDGE_LOOP('',(#2868));
#864=EDGE_LOOP('',(#2869));
#865=EDGE_LOOP('',(#2870,#2871,#2872,#2873));
#866=EDGE_LOOP('',(#2874));
#867=EDGE_LOOP('',(#2875));
#868=EDGE_LOOP('',(#2876,#2877,#2878,#2879));
#869=EDGE_LOOP('',(#2880,#2881,#2882,#2883));
#870=EDGE_LOOP('',(#2884,#2885,#2886,#2887));
#871=EDGE_LOOP('',(#2888,#2889,#2890,#2891));
#872=EDGE_LOOP('',(#2892,#2893,#2894,#2895));
#873=EDGE_LOOP('',(#2896,#2897,#2898,#2899));
#874=EDGE_LOOP('',(#2900,#2901,#2902,#2903));
#875=EDGE_LOOP('',(#2904,#2905,#2906,#2907));
#876=EDGE_LOOP('',(#2908,#2909,#2910,#2911));
#877=EDGE_LOOP('',(#2912,#2913,#2914,#2915));
#878=EDGE_LOOP('',(#2916,#2917,#2918,#2919));
#879=EDGE_LOOP('',(#2920,#2921,#2922,#2923));
#880=EDGE_LOOP('',(#2924,#2925,#2926,#2927));
#881=EDGE_LOOP('',(#2928));
#882=EDGE_LOOP('',(#2929));
#883=EDGE_LOOP('',(#2930,#2931,#2932,#2933));
#884=EDGE_LOOP('',(#2934));
#885=EDGE_LOOP('',(#2935));
#886=EDGE_LOOP('',(#2936,#2937,#2938,#2939));
#887=EDGE_LOOP('',(#2940,#2941,#2942,#2943));
#888=EDGE_LOOP('',(#2944,#2945,#2946,#2947));
#889=EDGE_LOOP('',(#2948,#2949,#2950,#2951));
#890=EDGE_LOOP('',(#2952,#2953,#2954,#2955));
#891=EDGE_LOOP('',(#2956,#2957,#2958,#2959));
#892=EDGE_LOOP('',(#2960,#2961,#2962,#2963));
#893=EDGE_LOOP('',(#2964,#2965,#2966,#2967,#2968));
#894=EDGE_LOOP('',(#2969,#2970,#2971,#2972));
#895=EDGE_LOOP('',(#2973,#2974,#2975,#2976));
#896=EDGE_LOOP('',(#2977,#2978,#2979,#2980));
#897=EDGE_LOOP('',(#2981,#2982,#2983,#2984));
#898=EDGE_LOOP('',(#2985,#2986,#2987,#2988));
#899=EDGE_LOOP('',(#2989,#2990,#2991,#2992));
#900=EDGE_LOOP('',(#2993,#2994));
#901=EDGE_LOOP('',(#2995));
#902=EDGE_LOOP('',(#2996,#2997,#2998,#2999,#3000));
#903=EDGE_LOOP('',(#3001,#3002));
#904=EDGE_LOOP('',(#3003));
#905=EDGE_LOOP('',(#3004,#3005,#3006,#3007,#3008,#3009));
#906=EDGE_LOOP('',(#3010,#3011,#3012,#3013));
#907=EDGE_LOOP('',(#3014,#3015,#3016,#3017,#3018,#3019));
#908=EDGE_LOOP('',(#3020,#3021,#3022,#3023));
#909=EDGE_LOOP('',(#3024,#3025,#3026,#3027));
#910=EDGE_LOOP('',(#3028,#3029,#3030,#3031));
#911=EDGE_LOOP('',(#3032,#3033,#3034,#3035));
#912=EDGE_LOOP('',(#3036,#3037,#3038,#3039));
#913=EDGE_LOOP('',(#3040,#3041,#3042,#3043,#3044,#3045,#3046));
#914=EDGE_LOOP('',(#3047,#3048,#3049,#3050,#3051,#3052,#3053));
#915=EDGE_LOOP('',(#3054,#3055,#3056,#3057,#3058,#3059,#3060));
#916=EDGE_LOOP('',(#3061,#3062,#3063,#3064,#3065,#3066,#3067));
#917=EDGE_LOOP('',(#3068,#3069,#3070,#3071));
#918=EDGE_LOOP('',(#3072,#3073,#3074,#3075));
#919=EDGE_LOOP('',(#3076));
#920=EDGE_LOOP('',(#3077));
#921=EDGE_LOOP('',(#3078,#3079,#3080,#3081));
#922=EDGE_LOOP('',(#3082,#3083,#3084,#3085,#3086));
#923=EDGE_LOOP('',(#3087,#3088,#3089,#3090));
#924=EDGE_LOOP('',(#3091,#3092,#3093,#3094));
#925=EDGE_LOOP('',(#3095,#3096,#3097,#3098));
#926=EDGE_LOOP('',(#3099,#3100,#3101,#3102));
#927=EDGE_LOOP('',(#3103,#3104,#3105,#3106));
#928=EDGE_LOOP('',(#3107,#3108,#3109,#3110));
#929=EDGE_LOOP('',(#3111,#3112));
#930=EDGE_LOOP('',(#3113));
#931=EDGE_LOOP('',(#3114,#3115,#3116,#3117,#3118));
#932=EDGE_LOOP('',(#3119,#3120));
#933=EDGE_LOOP('',(#3121));
#934=EDGE_LOOP('',(#3122,#3123,#3124,#3125,#3126,#3127));
#935=EDGE_LOOP('',(#3128,#3129,#3130,#3131));
#936=EDGE_LOOP('',(#3132,#3133,#3134,#3135,#3136,#3137));
#937=EDGE_LOOP('',(#3138,#3139,#3140,#3141));
#938=EDGE_LOOP('',(#3142,#3143,#3144,#3145));
#939=EDGE_LOOP('',(#3146,#3147,#3148,#3149));
#940=EDGE_LOOP('',(#3150,#3151,#3152,#3153));
#941=EDGE_LOOP('',(#3154,#3155,#3156,#3157));
#942=EDGE_LOOP('',(#3158,#3159,#3160,#3161,#3162,#3163,#3164));
#943=EDGE_LOOP('',(#3165,#3166,#3167,#3168,#3169,#3170,#3171));
#944=EDGE_LOOP('',(#3172,#3173,#3174,#3175,#3176,#3177,#3178));
#945=EDGE_LOOP('',(#3179,#3180,#3181,#3182,#3183,#3184,#3185));
#946=EDGE_LOOP('',(#3186,#3187,#3188,#3189));
#947=EDGE_LOOP('',(#3190,#3191,#3192,#3193));
#948=EDGE_LOOP('',(#3194));
#949=EDGE_LOOP('',(#3195));
#950=EDGE_LOOP('',(#3196,#3197,#3198,#3199));
#951=EDGE_LOOP('',(#3200,#3201,#3202,#3203));
#952=EDGE_LOOP('',(#3204,#3205,#3206,#3207));
#953=EDGE_LOOP('',(#3208,#3209));
#954=EDGE_LOOP('',(#3210));
#955=EDGE_LOOP('',(#3211,#3212,#3213,#3214));
#956=EDGE_LOOP('',(#3215,#3216,#3217,#3218));
#957=EDGE_LOOP('',(#3219,#3220));
#958=EDGE_LOOP('',(#3221));
#959=EDGE_LOOP('',(#3222,#3223,#3224,#3225));
#960=EDGE_LOOP('',(#3226,#3227,#3228,#3229));
#961=EDGE_LOOP('',(#3230,#3231,#3232,#3233));
#962=EDGE_LOOP('',(#3234,#3235,#3236,#3237));
#963=EDGE_LOOP('',(#3238,#3239,#3240,#3241));
#964=EDGE_LOOP('',(#3242,#3243,#3244,#3245));
#965=EDGE_LOOP('',(#3246,#3247,#3248,#3249,#3250,#3251,#3252,#3253,#3254,
#3255));
#966=EDGE_LOOP('',(#3256));
#967=EDGE_LOOP('',(#3257,#3258,#3259,#3260));
#968=EDGE_LOOP('',(#3261,#3262,#3263,#3264,#3265,#3266,#3267,#3268,#3269,
#3270));
#969=EDGE_LOOP('',(#3271));
#970=EDGE_LOOP('',(#3272,#3273,#3274,#3275));
#971=EDGE_LOOP('',(#3276));
#972=EDGE_LOOP('',(#3277));
#973=EDGE_LOOP('',(#3278,#3279,#3280,#3281,#3282,#3283,#3284,#3285));
#974=EDGE_LOOP('',(#3286,#3287,#3288,#3289));
#975=EDGE_LOOP('',(#3290,#3291,#3292,#3293));
#976=EDGE_LOOP('',(#3294,#3295,#3296,#3297));
#977=EDGE_LOOP('',(#3298,#3299,#3300,#3301));
#978=EDGE_LOOP('',(#3302,#3303,#3304,#3305,#3306,#3307,#3308,#3309));
#979=EDGE_LOOP('',(#3310,#3311,#3312,#3313));
#980=EDGE_LOOP('',(#3314,#3315,#3316,#3317));
#981=EDGE_LOOP('',(#3318,#3319,#3320,#3321));
#982=EDGE_LOOP('',(#3322,#3323,#3324,#3325));
#983=EDGE_LOOP('',(#3326));
#984=EDGE_LOOP('',(#3327,#3328,#3329,#3330));
#985=EDGE_LOOP('',(#3331,#3332,#3333,#3334));
#986=EDGE_LOOP('',(#3335,#3336,#3337,#3338));
#987=EDGE_LOOP('',(#3339));
#988=EDGE_LOOP('',(#3340));
#989=EDGE_LOOP('',(#3341,#3342,#3343,#3344));
#990=EDGE_LOOP('',(#3345,#3346,#3347,#3348));
#991=EDGE_LOOP('',(#3349,#3350,#3351,#3352));
#992=EDGE_LOOP('',(#3353));
#993=EDGE_LOOP('',(#3354,#3355,#3356,#3357));
#994=EDGE_LOOP('',(#3358,#3359,#3360,#3361));
#995=EDGE_LOOP('',(#3362,#3363,#3364,#3365));
#996=EDGE_LOOP('',(#3366,#3367,#3368,#3369));
#997=EDGE_LOOP('',(#3370,#3371,#3372,#3373));
#998=EDGE_LOOP('',(#3374,#3375,#3376,#3377));
#999=EDGE_LOOP('',(#3378,#3379,#3380,#3381,#3382,#3383));
#1000=EDGE_LOOP('',(#3384,#3385,#3386,#3387,#3388,#3389));
#1001=EDGE_LOOP('',(#3390));
#1002=EDGE_LOOP('',(#3391,#3392,#3393,#3394));
#1003=EDGE_LOOP('',(#3395,#3396,#3397,#3398));
#1004=EDGE_LOOP('',(#3399,#3400,#3401,#3402));
#1005=EDGE_LOOP('',(#3403));
#1006=EDGE_LOOP('',(#3404));
#1007=EDGE_LOOP('',(#3405,#3406,#3407,#3408));
#1008=EDGE_LOOP('',(#3409,#3410,#3411,#3412));
#1009=EDGE_LOOP('',(#3413,#3414,#3415,#3416));
#1010=EDGE_LOOP('',(#3417));
#1011=EDGE_LOOP('',(#3418,#3419,#3420,#3421));
#1012=EDGE_LOOP('',(#3422,#3423,#3424,#3425));
#1013=EDGE_LOOP('',(#3426,#3427,#3428,#3429));
#1014=EDGE_LOOP('',(#3430,#3431,#3432,#3433));
#1015=EDGE_LOOP('',(#3434,#3435,#3436,#3437));
#1016=EDGE_LOOP('',(#3438,#3439,#3440,#3441));
#1017=EDGE_LOOP('',(#3442,#3443,#3444,#3445,#3446,#3447));
#1018=EDGE_LOOP('',(#3448,#3449,#3450,#3451,#3452,#3453));
#1019=EDGE_LOOP('',(#3454,#3455,#3456,#3457));
#1020=EDGE_LOOP('',(#3458,#3459,#3460,#3461));
#1021=EDGE_LOOP('',(#3462));
#1022=EDGE_LOOP('',(#3463));
#1023=EDGE_LOOP('',(#3464));
#1024=EDGE_LOOP('',(#3465));
#1025=EDGE_LOOP('',(#3466,#3467,#3468,#3469,#3470,#3471,#3472,#3473,#3474));
#1026=EDGE_LOOP('',(#3475,#3476,#3477,#3478,#3479,#3480,#3481,#3482,#3483));
#1027=EDGE_LOOP('',(#3484,#3485,#3486,#3487));
#1028=EDGE_LOOP('',(#3488,#3489,#3490,#3491));
#1029=EDGE_LOOP('',(#3492,#3493,#3494,#3495));
#1030=EDGE_LOOP('',(#3496,#3497,#3498,#3499));
#1031=EDGE_LOOP('',(#3500,#3501,#3502,#3503));
#1032=EDGE_LOOP('',(#3504,#3505,#3506,#3507));
#1033=EDGE_LOOP('',(#3508,#3509,#3510,#3511));
#1034=EDGE_LOOP('',(#3512));
#1035=EDGE_LOOP('',(#3513));
#1036=EDGE_LOOP('',(#3514));
#1037=EDGE_LOOP('',(#3515));
#1038=EDGE_LOOP('',(#3516,#3517,#3518,#3519));
#1039=EDGE_LOOP('',(#3520,#3521,#3522,#3523));
#1040=EDGE_LOOP('',(#3524,#3525,#3526,#3527));
#1041=EDGE_LOOP('',(#3528,#3529,#3530,#3531));
#1042=EDGE_LOOP('',(#3532,#3533,#3534,#3535));
#1043=EDGE_LOOP('',(#3536,#3537,#3538,#3539));
#1044=EDGE_LOOP('',(#3540,#3541,#3542,#3543));
#1045=EDGE_LOOP('',(#3544,#3545,#3546,#3547));
#1046=EDGE_LOOP('',(#3548,#3549,#3550,#3551));
#1047=EDGE_LOOP('',(#3552));
#1048=EDGE_LOOP('',(#3553));
#1049=EDGE_LOOP('',(#3554));
#1050=EDGE_LOOP('',(#3555));
#1051=EDGE_LOOP('',(#3556,#3557,#3558,#3559));
#1052=EDGE_LOOP('',(#3560));
#1053=EDGE_LOOP('',(#3561));
#1054=EDGE_LOOP('',(#3562));
#1055=EDGE_LOOP('',(#3563));
#1056=EDGE_LOOP('',(#3564,#3565,#3566,#3567));
#1057=EDGE_LOOP('',(#3568));
#1058=EDGE_LOOP('',(#3569,#3570,#3571,#3572));
#1059=EDGE_LOOP('',(#3573));
#1060=EDGE_LOOP('',(#3574,#3575,#3576,#3577));
#1061=EDGE_LOOP('',(#3578,#3579,#3580,#3581));
#1062=EDGE_LOOP('',(#3582,#3583,#3584,#3585));
#1063=EDGE_LOOP('',(#3586,#3587,#3588,#3589));
#1064=EDGE_LOOP('',(#3590,#3591,#3592,#3593));
#1065=EDGE_LOOP('',(#3594,#3595,#3596,#3597));
#1066=EDGE_LOOP('',(#3598));
#1067=EDGE_LOOP('',(#3599));
#1068=EDGE_LOOP('',(#3600,#3601,#3602,#3603));
#1069=EDGE_LOOP('',(#3604));
#1070=EDGE_LOOP('',(#3605));
#1071=EDGE_LOOP('',(#3606,#3607,#3608,#3609));
#1072=EDGE_LOOP('',(#3610));
#1073=EDGE_LOOP('',(#3611));
#1074=EDGE_LOOP('',(#3612,#3613,#3614,#3615));
#1075=EDGE_LOOP('',(#3616,#3617,#3618,#3619));
#1076=EDGE_LOOP('',(#3620,#3621,#3622,#3623));
#1077=EDGE_LOOP('',(#3624,#3625,#3626,#3627));
#1078=EDGE_LOOP('',(#3628,#3629,#3630,#3631));
#1079=EDGE_LOOP('',(#3632,#3633,#3634,#3635));
#1080=EDGE_LOOP('',(#3636,#3637,#3638,#3639,#3640,#3641));
#1081=EDGE_LOOP('',(#3642,#3643,#3644,#3645,#3646,#3647));
#1082=EDGE_LOOP('',(#3648));
#1083=EDGE_LOOP('',(#3649));
#1084=EDGE_LOOP('',(#3650,#3651,#3652,#3653));
#1085=EDGE_LOOP('',(#3654,#3655,#3656,#3657));
#1086=EDGE_LOOP('',(#3658,#3659,#3660,#3661));
#1087=EDGE_LOOP('',(#3662));
#1088=EDGE_LOOP('',(#3663));
#1089=EDGE_LOOP('',(#3664,#3665,#3666,#3667));
#1090=EDGE_LOOP('',(#3668,#3669,#3670,#3671));
#1091=EDGE_LOOP('',(#3672,#3673,#3674,#3675));
#1092=EDGE_LOOP('',(#3676,#3677,#3678,#3679));
#1093=EDGE_LOOP('',(#3680));
#1094=EDGE_LOOP('',(#3681));
#1095=EDGE_LOOP('',(#3682));
#1096=EDGE_LOOP('',(#3683));
#1097=EDGE_LOOP('',(#3684,#3685,#3686,#3687,#3688,#3689,#3690,#3691,#3692));
#1098=EDGE_LOOP('',(#3693,#3694,#3695,#3696,#3697,#3698,#3699,#3700,#3701));
#1099=EDGE_LOOP('',(#3702,#3703,#3704,#3705));
#1100=EDGE_LOOP('',(#3706,#3707,#3708,#3709));
#1101=EDGE_LOOP('',(#3710,#3711,#3712,#3713));
#1102=EDGE_LOOP('',(#3714,#3715,#3716,#3717));
#1103=EDGE_LOOP('',(#3718,#3719,#3720,#3721));
#1104=EDGE_LOOP('',(#3722,#3723,#3724,#3725));
#1105=EDGE_LOOP('',(#3726,#3727,#3728,#3729));
#1106=EDGE_LOOP('',(#3730));
#1107=EDGE_LOOP('',(#3731));
#1108=EDGE_LOOP('',(#3732));
#1109=EDGE_LOOP('',(#3733));
#1110=EDGE_LOOP('',(#3734,#3735,#3736,#3737));
#1111=EDGE_LOOP('',(#3738));
#1112=EDGE_LOOP('',(#3739));
#1113=LINE('',#6092,#1478);
#1114=LINE('',#6094,#1479);
#1115=LINE('',#6096,#1480);
#1116=LINE('',#6097,#1481);
#1117=LINE('',#6100,#1482);
#1118=LINE('',#6102,#1483);
#1119=LINE('',#6103,#1484);
#1120=LINE('',#6106,#1485);
#1121=LINE('',#6108,#1486);
#1122=LINE('',#6109,#1487);
#1123=LINE('',#6111,#1488);
#1124=LINE('',#6112,#1489);
#1125=LINE('',#6117,#1490);
#1126=LINE('',#6119,#1491);
#1127=LINE('',#6121,#1492);
#1128=LINE('',#6122,#1493);
#1129=LINE('',#6125,#1494);
#1130=LINE('',#6127,#1495);
#1131=LINE('',#6128,#1496);
#1132=LINE('',#6131,#1497);
#1133=LINE('',#6133,#1498);
#1134=LINE('',#6134,#1499);
#1135=LINE('',#6136,#1500);
#1136=LINE('',#6137,#1501);
#1137=LINE('',#6143,#1502);
#1138=LINE('',#6149,#1503);
#1139=LINE('',#6155,#1504);
#1140=LINE('',#6161,#1505);
#1141=LINE('',#6167,#1506);
#1142=LINE('',#6173,#1507);
#1143=LINE('',#6179,#1508);
#1144=LINE('',#6185,#1509);
#1145=LINE('',#6191,#1510);
#1146=LINE('',#6197,#1511);
#1147=LINE('',#6203,#1512);
#1148=LINE('',#6209,#1513);
#1149=LINE('',#6214,#1514);
#1150=LINE('',#6216,#1515);
#1151=LINE('',#6218,#1516);
#1152=LINE('',#6219,#1517);
#1153=LINE('',#6222,#1518);
#1154=LINE('',#6224,#1519);
#1155=LINE('',#6225,#1520);
#1156=LINE('',#6228,#1521);
#1157=LINE('',#6230,#1522);
#1158=LINE('',#6231,#1523);
#1159=LINE('',#6233,#1524);
#1160=LINE('',#6234,#1525);
#1161=LINE('',#6242,#1526);
#1162=LINE('',#6248,#1527);
#1163=LINE('',#6253,#1528);
#1164=LINE('',#6255,#1529);
#1165=LINE('',#6257,#1530);
#1166=LINE('',#6258,#1531);
#1167=LINE('',#6261,#1532);
#1168=LINE('',#6263,#1533);
#1169=LINE('',#6264,#1534);
#1170=LINE('',#6267,#1535);
#1171=LINE('',#6269,#1536);
#1172=LINE('',#6270,#1537);
#1173=LINE('',#6272,#1538);
#1174=LINE('',#6273,#1539);
#1175=LINE('',#6280,#1540);
#1176=LINE('',#6282,#1541);
#1177=LINE('',#6284,#1542);
#1178=LINE('',#6285,#1543);
#1179=LINE('',#6288,#1544);
#1180=LINE('',#6290,#1545);
#1181=LINE('',#6291,#1546);
#1182=LINE('',#6294,#1547);
#1183=LINE('',#6296,#1548);
#1184=LINE('',#6297,#1549);
#1185=LINE('',#6299,#1550);
#1186=LINE('',#6300,#1551);
#1187=LINE('',#6308,#1552);
#1188=LINE('',#6314,#1553);
#1189=LINE('',#6319,#1554);
#1190=LINE('',#6321,#1555);
#1191=LINE('',#6323,#1556);
#1192=LINE('',#6324,#1557);
#1193=LINE('',#6327,#1558);
#1194=LINE('',#6329,#1559);
#1195=LINE('',#6330,#1560);
#1196=LINE('',#6333,#1561);
#1197=LINE('',#6335,#1562);
#1198=LINE('',#6336,#1563);
#1199=LINE('',#6338,#1564);
#1200=LINE('',#6339,#1565);
#1201=LINE('',#6346,#1566);
#1202=LINE('',#6348,#1567);
#1203=LINE('',#6350,#1568);
#1204=LINE('',#6351,#1569);
#1205=LINE('',#6354,#1570);
#1206=LINE('',#6356,#1571);
#1207=LINE('',#6357,#1572);
#1208=LINE('',#6360,#1573);
#1209=LINE('',#6362,#1574);
#1210=LINE('',#6363,#1575);
#1211=LINE('',#6365,#1576);
#1212=LINE('',#6366,#1577);
#1213=LINE('',#6373,#1578);
#1214=LINE('',#6377,#1579);
#1215=LINE('',#6382,#1580);
#1216=LINE('',#6386,#1581);
#1217=LINE('',#6393,#1582);
#1218=LINE('',#6395,#1583);
#1219=LINE('',#6397,#1584);
#1220=LINE('',#6398,#1585);
#1221=LINE('',#6401,#1586);
#1222=LINE('',#6403,#1587);
#1223=LINE('',#6404,#1588);
#1224=LINE('',#6407,#1589);
#1225=LINE('',#6409,#1590);
#1226=LINE('',#6410,#1591);
#1227=LINE('',#6412,#1592);
#1228=LINE('',#6413,#1593);
#1229=LINE('',#6417,#1594);
#1230=LINE('',#6426,#1595);
#1231=LINE('',#6433,#1596);
#1232=LINE('',#6435,#1597);
#1233=LINE('',#6437,#1598);
#1234=LINE('',#6439,#1599);
#1235=LINE('',#6440,#1600);
#1236=LINE('',#6443,#1601);
#1237=LINE('',#6444,#1602);
#1238=LINE('',#6447,#1603);
#1239=LINE('',#6448,#1604);
#1240=LINE('',#6450,#1605);
#1241=LINE('',#6451,#1606);
#1242=LINE('',#6454,#1607);
#1243=LINE('',#6455,#1608);
#1244=LINE('',#6459,#1609);
#1245=LINE('',#6463,#1610);
#1246=LINE('',#6466,#1611);
#1247=LINE('',#6467,#1612);
#1248=LINE('',#6470,#1613);
#1249=LINE('',#6471,#1614);
#1250=LINE('',#6474,#1615);
#1251=LINE('',#6476,#1616);
#1252=LINE('',#6477,#1617);
#1253=LINE('',#6480,#1618);
#1254=LINE('',#6481,#1619);
#1255=LINE('',#6484,#1620);
#1256=LINE('',#6485,#1621);
#1257=LINE('',#6487,#1622);
#1258=LINE('',#6493,#1623);
#1259=LINE('',#6497,#1624);
#1260=LINE('',#6502,#1625);
#1261=LINE('',#6506,#1626);
#1262=LINE('',#6513,#1627);
#1263=LINE('',#6515,#1628);
#1264=LINE('',#6517,#1629);
#1265=LINE('',#6518,#1630);
#1266=LINE('',#6521,#1631);
#1267=LINE('',#6523,#1632);
#1268=LINE('',#6524,#1633);
#1269=LINE('',#6527,#1634);
#1270=LINE('',#6529,#1635);
#1271=LINE('',#6530,#1636);
#1272=LINE('',#6532,#1637);
#1273=LINE('',#6533,#1638);
#1274=LINE('',#6537,#1639);
#1275=LINE('',#6546,#1640);
#1276=LINE('',#6553,#1641);
#1277=LINE('',#6555,#1642);
#1278=LINE('',#6557,#1643);
#1279=LINE('',#6559,#1644);
#1280=LINE('',#6560,#1645);
#1281=LINE('',#6563,#1646);
#1282=LINE('',#6564,#1647);
#1283=LINE('',#6567,#1648);
#1284=LINE('',#6568,#1649);
#1285=LINE('',#6570,#1650);
#1286=LINE('',#6571,#1651);
#1287=LINE('',#6574,#1652);
#1288=LINE('',#6575,#1653);
#1289=LINE('',#6579,#1654);
#1290=LINE('',#6583,#1655);
#1291=LINE('',#6586,#1656);
#1292=LINE('',#6587,#1657);
#1293=LINE('',#6590,#1658);
#1294=LINE('',#6591,#1659);
#1295=LINE('',#6594,#1660);
#1296=LINE('',#6596,#1661);
#1297=LINE('',#6597,#1662);
#1298=LINE('',#6600,#1663);
#1299=LINE('',#6601,#1664);
#1300=LINE('',#6604,#1665);
#1301=LINE('',#6605,#1666);
#1302=LINE('',#6607,#1667);
#1303=LINE('',#6614,#1668);
#1304=LINE('',#6619,#1669);
#1305=LINE('',#6623,#1670);
#1306=LINE('',#6626,#1671);
#1307=LINE('',#6628,#1672);
#1308=LINE('',#6636,#1673);
#1309=LINE('',#6640,#1674);
#1310=LINE('',#6643,#1675);
#1311=LINE('',#6645,#1676);
#1312=LINE('',#6652,#1677);
#1313=LINE('',#6654,#1678);
#1314=LINE('',#6655,#1679);
#1315=LINE('',#6657,#1680);
#1316=LINE('',#6658,#1681);
#1317=LINE('',#6661,#1682);
#1318=LINE('',#6663,#1683);
#1319=LINE('',#6664,#1684);
#1320=LINE('',#6668,#1685);
#1321=LINE('',#6672,#1686);
#1322=LINE('',#6676,#1687);
#1323=LINE('',#6677,#1688);
#1324=LINE('',#6678,#1689);
#1325=LINE('',#6681,#1690);
#1326=LINE('',#6682,#1691);
#1327=LINE('',#6685,#1692);
#1328=LINE('',#6686,#1693);
#1329=LINE('',#6688,#1694);
#1330=LINE('',#6694,#1695);
#1331=LINE('',#6696,#1696);
#1332=LINE('',#6698,#1697);
#1333=LINE('',#6700,#1698);
#1334=LINE('',#6702,#1699);
#1335=LINE('',#6704,#1700);
#1336=LINE('',#6706,#1701);
#1337=LINE('',#6707,#1702);
#1338=LINE('',#6710,#1703);
#1339=LINE('',#6712,#1704);
#1340=LINE('',#6713,#1705);
#1341=LINE('',#6716,#1706);
#1342=LINE('',#6717,#1707);
#1343=LINE('',#6720,#1708);
#1344=LINE('',#6721,#1709);
#1345=LINE('',#6724,#1710);
#1346=LINE('',#6725,#1711);
#1347=LINE('',#6729,#1712);
#1348=LINE('',#6730,#1713);
#1349=LINE('',#6732,#1714);
#1350=LINE('',#6733,#1715);
#1351=LINE('',#6735,#1716);
#1352=LINE('',#6737,#1717);
#1353=LINE('',#6739,#1718);
#1354=LINE('',#6748,#1719);
#1355=LINE('',#6752,#1720);
#1356=LINE('',#6756,#1721);
#1357=LINE('',#6763,#1722);
#1358=LINE('',#6767,#1723);
#1359=LINE('',#6771,#1724);
#1360=LINE('',#6776,#1725);
#1361=LINE('',#6778,#1726);
#1362=LINE('',#6780,#1727);
#1363=LINE('',#6781,#1728);
#1364=LINE('',#6784,#1729);
#1365=LINE('',#6786,#1730);
#1366=LINE('',#6787,#1731);
#1367=LINE('',#6790,#1732);
#1368=LINE('',#6792,#1733);
#1369=LINE('',#6793,#1734);
#1370=LINE('',#6796,#1735);
#1371=LINE('',#6798,#1736);
#1372=LINE('',#6799,#1737);
#1373=LINE('',#6802,#1738);
#1374=LINE('',#6804,#1739);
#1375=LINE('',#6805,#1740);
#1376=LINE('',#6807,#1741);
#1377=LINE('',#6808,#1742);
#1378=LINE('',#6818,#1743);
#1379=LINE('',#6822,#1744);
#1380=LINE('',#6826,#1745);
#1381=LINE('',#6833,#1746);
#1382=LINE('',#6837,#1747);
#1383=LINE('',#6841,#1748);
#1384=LINE('',#6846,#1749);
#1385=LINE('',#6848,#1750);
#1386=LINE('',#6850,#1751);
#1387=LINE('',#6851,#1752);
#1388=LINE('',#6854,#1753);
#1389=LINE('',#6856,#1754);
#1390=LINE('',#6857,#1755);
#1391=LINE('',#6860,#1756);
#1392=LINE('',#6862,#1757);
#1393=LINE('',#6863,#1758);
#1394=LINE('',#6866,#1759);
#1395=LINE('',#6868,#1760);
#1396=LINE('',#6869,#1761);
#1397=LINE('',#6872,#1762);
#1398=LINE('',#6874,#1763);
#1399=LINE('',#6875,#1764);
#1400=LINE('',#6877,#1765);
#1401=LINE('',#6878,#1766);
#1402=LINE('',#6886,#1767);
#1403=LINE('',#6892,#1768);
#1404=LINE('',#6908,#1769);
#1405=LINE('',#6929,#1770);
#1406=LINE('',#6954,#1771);
#1407=LINE('',#6955,#1772);
#1408=LINE('',#6957,#1773);
#1409=LINE('',#6959,#1774);
#1410=LINE('',#6964,#1775);
#1411=LINE('',#6967,#1776);
#1412=LINE('',#6969,#1777);
#1413=LINE('',#7002,#1778);
#1414=LINE('',#7008,#1779);
#1415=LINE('',#7014,#1780);
#1416=LINE('',#7020,#1781);
#1417=LINE('',#7025,#1782);
#1418=LINE('',#7027,#1783);
#1419=LINE('',#7029,#1784);
#1420=LINE('',#7030,#1785);
#1421=LINE('',#7033,#1786);
#1422=LINE('',#7035,#1787);
#1423=LINE('',#7036,#1788);
#1424=LINE('',#7039,#1789);
#1425=LINE('',#7041,#1790);
#1426=LINE('',#7042,#1791);
#1427=LINE('',#7044,#1792);
#1428=LINE('',#7045,#1793);
#1429=LINE('',#7053,#1794);
#1430=LINE('',#7060,#1795);
#1431=LINE('',#7066,#1796);
#1432=LINE('',#7070,#1797);
#1433=LINE('',#7074,#1798);
#1434=LINE('',#7076,#1799);
#1435=LINE('',#7077,#1800);
#1436=LINE('',#7080,#1801);
#1437=LINE('',#7081,#1802);
#1438=LINE('',#7084,#1803);
#1439=LINE('',#7085,#1804);
#1440=LINE('',#7087,#1805);
#1441=LINE('',#7094,#1806);
#1442=LINE('',#7103,#1807);
#1443=LINE('',#7111,#1808);
#1444=LINE('',#7113,#1809);
#1445=LINE('',#7115,#1810);
#1446=LINE('',#7116,#1811);
#1447=LINE('',#7119,#1812);
#1448=LINE('',#7121,#1813);
#1449=LINE('',#7122,#1814);
#1450=LINE('',#7125,#1815);
#1451=LINE('',#7127,#1816);
#1452=LINE('',#7128,#1817);
#1453=LINE('',#7131,#1818);
#1454=LINE('',#7133,#1819);
#1455=LINE('',#7134,#1820);
#1456=LINE('',#7137,#1821);
#1457=LINE('',#7139,#1822);
#1458=LINE('',#7140,#1823);
#1459=LINE('',#7142,#1824);
#1460=LINE('',#7143,#1825);
#1461=LINE('',#7155,#1826);
#1462=LINE('',#7159,#1827);
#1463=LINE('',#7163,#1828);
#1464=LINE('',#7170,#1829);
#1465=LINE('',#7172,#1830);
#1466=LINE('',#7178,#1831);
#1467=LINE('',#7184,#1832);
#1468=LINE('',#7200,#1833);
#1469=LINE('',#7221,#1834);
#1470=LINE('',#7246,#1835);
#1471=LINE('',#7247,#1836);
#1472=LINE('',#7249,#1837);
#1473=LINE('',#7251,#1838);
#1474=LINE('',#7256,#1839);
#1475=LINE('',#7259,#1840);
#1476=LINE('',#7261,#1841);
#1477=LINE('',#7285,#1842);
#1478=VECTOR('',#4851,1.);
#1479=VECTOR('',#4852,1.);
#1480=VECTOR('',#4853,1.);
#1481=VECTOR('',#4854,1.);
#1482=VECTOR('',#4857,1.);
#1483=VECTOR('',#4858,1.);
#1484=VECTOR('',#4859,1.);
#1485=VECTOR('',#4862,1.);
#1486=VECTOR('',#4863,1.);
#1487=VECTOR('',#4864,1.);
#1488=VECTOR('',#4867,1.);
#1489=VECTOR('',#4868,1.);
#1490=VECTOR('',#4873,1.);
#1491=VECTOR('',#4874,1.);
#1492=VECTOR('',#4875,1.);
#1493=VECTOR('',#4876,1.);
#1494=VECTOR('',#4879,1.);
#1495=VECTOR('',#4880,1.);
#1496=VECTOR('',#4881,1.);
#1497=VECTOR('',#4884,1.);
#1498=VECTOR('',#4885,1.);
#1499=VECTOR('',#4886,1.);
#1500=VECTOR('',#4889,1.);
#1501=VECTOR('',#4890,1.);
#1502=VECTOR('',#4897,0.274999999999999);
#1503=VECTOR('',#4904,0.275);
#1504=VECTOR('',#4911,0.275);
#1505=VECTOR('',#4918,0.274999999999999);
#1506=VECTOR('',#4925,0.34);
#1507=VECTOR('',#4932,0.34);
#1508=VECTOR('',#4939,0.25);
#1509=VECTOR('',#4946,0.25);
#1510=VECTOR('',#4953,0.25);
#1511=VECTOR('',#4960,0.25);
#1512=VECTOR('',#4967,0.25);
#1513=VECTOR('',#4974,0.25);
#1514=VECTOR('',#4979,1.);
#1515=VECTOR('',#4980,1.);
#1516=VECTOR('',#4981,1.);
#1517=VECTOR('',#4982,1.);
#1518=VECTOR('',#4985,1.);
#1519=VECTOR('',#4986,1.);
#1520=VECTOR('',#4987,1.);
#1521=VECTOR('',#4990,1.);
#1522=VECTOR('',#4991,1.);
#1523=VECTOR('',#4992,1.);
#1524=VECTOR('',#4995,1.);
#1525=VECTOR('',#4996,1.);
#1526=VECTOR('',#5007,0.21);
#1527=VECTOR('',#5014,0.21);
#1528=VECTOR('',#5019,1.);
#1529=VECTOR('',#5020,1.);
#1530=VECTOR('',#5021,1.);
#1531=VECTOR('',#5022,1.);
#1532=VECTOR('',#5025,1.);
#1533=VECTOR('',#5026,1.);
#1534=VECTOR('',#5027,1.);
#1535=VECTOR('',#5030,1.);
#1536=VECTOR('',#5031,1.);
#1537=VECTOR('',#5032,1.);
#1538=VECTOR('',#5035,1.);
#1539=VECTOR('',#5036,1.);
#1540=VECTOR('',#5045,1.);
#1541=VECTOR('',#5046,1.);
#1542=VECTOR('',#5047,1.);
#1543=VECTOR('',#5048,1.);
#1544=VECTOR('',#5051,1.);
#1545=VECTOR('',#5052,1.);
#1546=VECTOR('',#5053,1.);
#1547=VECTOR('',#5056,1.);
#1548=VECTOR('',#5057,1.);
#1549=VECTOR('',#5058,1.);
#1550=VECTOR('',#5061,1.);
#1551=VECTOR('',#5062,1.);
#1552=VECTOR('',#5073,0.210000000000001);
#1553=VECTOR('',#5080,0.210000000000001);
#1554=VECTOR('',#5085,1.);
#1555=VECTOR('',#5086,1.);
#1556=VECTOR('',#5087,1.);
#1557=VECTOR('',#5088,1.);
#1558=VECTOR('',#5091,1.);
#1559=VECTOR('',#5092,1.);
#1560=VECTOR('',#5093,1.);
#1561=VECTOR('',#5096,1.);
#1562=VECTOR('',#5097,1.);
#1563=VECTOR('',#5098,1.);
#1564=VECTOR('',#5101,1.);
#1565=VECTOR('',#5102,1.);
#1566=VECTOR('',#5111,1.);
#1567=VECTOR('',#5112,1.);
#1568=VECTOR('',#5113,1.);
#1569=VECTOR('',#5114,1.);
#1570=VECTOR('',#5117,1.);
#1571=VECTOR('',#5118,1.);
#1572=VECTOR('',#5119,1.);
#1573=VECTOR('',#5122,1.);
#1574=VECTOR('',#5123,1.);
#1575=VECTOR('',#5124,1.);
#1576=VECTOR('',#5127,1.);
#1577=VECTOR('',#5128,1.);
#1578=VECTOR('',#5137,0.5);
#1579=VECTOR('',#5140,1.);
#1580=VECTOR('',#5145,0.5);
#1581=VECTOR('',#5148,1.);
#1582=VECTOR('',#5155,1.);
#1583=VECTOR('',#5156,1.);
#1584=VECTOR('',#5157,1.);
#1585=VECTOR('',#5158,1.);
#1586=VECTOR('',#5161,1.);
#1587=VECTOR('',#5162,1.);
#1588=VECTOR('',#5163,1.);
#1589=VECTOR('',#5166,1.);
#1590=VECTOR('',#5167,1.);
#1591=VECTOR('',#5168,1.);
#1592=VECTOR('',#5171,1.);
#1593=VECTOR('',#5172,1.);
#1594=VECTOR('',#5179,1.);
#1595=VECTOR('',#5192,1.);
#1596=VECTOR('',#5201,1.);
#1597=VECTOR('',#5202,1.);
#1598=VECTOR('',#5203,1.);
#1599=VECTOR('',#5204,1.);
#1600=VECTOR('',#5205,1.);
#1601=VECTOR('',#5208,1.);
#1602=VECTOR('',#5209,1.);
#1603=VECTOR('',#5212,1.);
#1604=VECTOR('',#5213,1.);
#1605=VECTOR('',#5214,1.);
#1606=VECTOR('',#5215,1.);
#1607=VECTOR('',#5218,1.);
#1608=VECTOR('',#5219,1.);
#1609=VECTOR('',#5224,0.33);
#1610=VECTOR('',#5229,0.33);
#1611=VECTOR('',#5232,1.);
#1612=VECTOR('',#5233,1.);
#1613=VECTOR('',#5236,1.);
#1614=VECTOR('',#5237,1.);
#1615=VECTOR('',#5240,1.);
#1616=VECTOR('',#5241,1.);
#1617=VECTOR('',#5242,1.);
#1618=VECTOR('',#5245,1.);
#1619=VECTOR('',#5246,1.);
#1620=VECTOR('',#5249,1.);
#1621=VECTOR('',#5250,1.);
#1622=VECTOR('',#5253,1.);
#1623=VECTOR('',#5260,0.5);
#1624=VECTOR('',#5263,1.);
#1625=VECTOR('',#5268,0.5);
#1626=VECTOR('',#5271,1.);
#1627=VECTOR('',#5278,1.);
#1628=VECTOR('',#5279,1.);
#1629=VECTOR('',#5280,1.);
#1630=VECTOR('',#5281,1.);
#1631=VECTOR('',#5284,1.);
#1632=VECTOR('',#5285,1.);
#1633=VECTOR('',#5286,1.);
#1634=VECTOR('',#5289,1.);
#1635=VECTOR('',#5290,1.);
#1636=VECTOR('',#5291,1.);
#1637=VECTOR('',#5294,1.);
#1638=VECTOR('',#5295,1.);
#1639=VECTOR('',#5302,1.);
#1640=VECTOR('',#5315,1.);
#1641=VECTOR('',#5324,1.);
#1642=VECTOR('',#5325,1.);
#1643=VECTOR('',#5326,1.);
#1644=VECTOR('',#5327,1.);
#1645=VECTOR('',#5328,1.);
#1646=VECTOR('',#5331,1.);
#1647=VECTOR('',#5332,1.);
#1648=VECTOR('',#5335,1.);
#1649=VECTOR('',#5336,1.);
#1650=VECTOR('',#5337,1.);
#1651=VECTOR('',#5338,1.);
#1652=VECTOR('',#5341,1.);
#1653=VECTOR('',#5342,1.);
#1654=VECTOR('',#5347,0.33);
#1655=VECTOR('',#5352,0.33);
#1656=VECTOR('',#5355,1.);
#1657=VECTOR('',#5356,1.);
#1658=VECTOR('',#5359,1.);
#1659=VECTOR('',#5360,1.);
#1660=VECTOR('',#5363,1.);
#1661=VECTOR('',#5364,1.);
#1662=VECTOR('',#5365,1.);
#1663=VECTOR('',#5368,1.);
#1664=VECTOR('',#5369,1.);
#1665=VECTOR('',#5372,1.);
#1666=VECTOR('',#5373,1.);
#1667=VECTOR('',#5376,1.);
#1668=VECTOR('',#5385,0.21);
#1669=VECTOR('',#5390,1.);
#1670=VECTOR('',#5393,1.);
#1671=VECTOR('',#5398,1.);
#1672=VECTOR('',#5401,1.);
#1673=VECTOR('',#5410,1.);
#1674=VECTOR('',#5413,1.);
#1675=VECTOR('',#5418,1.);
#1676=VECTOR('',#5421,1.);
#1677=VECTOR('',#5430,1.);
#1678=VECTOR('',#5431,1.);
#1679=VECTOR('',#5432,1.);
#1680=VECTOR('',#5435,1.);
#1681=VECTOR('',#5436,1.);
#1682=VECTOR('',#5439,1.);
#1683=VECTOR('',#5440,1.);
#1684=VECTOR('',#5441,1.);
#1685=VECTOR('',#5446,0.33);
#1686=VECTOR('',#5451,0.33);
#1687=VECTOR('',#5454,1.);
#1688=VECTOR('',#5455,1.);
#1689=VECTOR('',#5456,1.);
#1690=VECTOR('',#5459,1.);
#1691=VECTOR('',#5460,1.);
#1692=VECTOR('',#5463,1.);
#1693=VECTOR('',#5464,1.);
#1694=VECTOR('',#5467,1.);
#1695=VECTOR('',#5474,1.);
#1696=VECTOR('',#5475,1.);
#1697=VECTOR('',#5476,1.);
#1698=VECTOR('',#5477,1.);
#1699=VECTOR('',#5478,1.);
#1700=VECTOR('',#5479,1.);
#1701=VECTOR('',#5480,1.);
#1702=VECTOR('',#5481,1.);
#1703=VECTOR('',#5484,1.);
#1704=VECTOR('',#5485,1.);
#1705=VECTOR('',#5486,1.);
#1706=VECTOR('',#5489,1.);
#1707=VECTOR('',#5490,1.);
#1708=VECTOR('',#5493,1.);
#1709=VECTOR('',#5494,1.);
#1710=VECTOR('',#5497,1.);
#1711=VECTOR('',#5498,1.);
#1712=VECTOR('',#5501,1.);
#1713=VECTOR('',#5502,1.);
#1714=VECTOR('',#5503,1.);
#1715=VECTOR('',#5504,1.);
#1716=VECTOR('',#5507,1.);
#1717=VECTOR('',#5510,1.);
#1718=VECTOR('',#5513,1.);
#1719=VECTOR('',#5526,0.475);
#1720=VECTOR('',#5531,0.5);
#1721=VECTOR('',#5536,0.485);
#1722=VECTOR('',#5545,0.31);
#1723=VECTOR('',#5550,0.3);
#1724=VECTOR('',#5555,0.27);
#1725=VECTOR('',#5560,1.);
#1726=VECTOR('',#5561,1.);
#1727=VECTOR('',#5562,1.);
#1728=VECTOR('',#5563,1.);
#1729=VECTOR('',#5566,1.);
#1730=VECTOR('',#5567,1.);
#1731=VECTOR('',#5568,1.);
#1732=VECTOR('',#5571,1.);
#1733=VECTOR('',#5572,1.);
#1734=VECTOR('',#5573,1.);
#1735=VECTOR('',#5576,1.);
#1736=VECTOR('',#5577,1.);
#1737=VECTOR('',#5578,1.);
#1738=VECTOR('',#5581,1.);
#1739=VECTOR('',#5582,1.);
#1740=VECTOR('',#5583,1.);
#1741=VECTOR('',#5586,1.);
#1742=VECTOR('',#5587,1.);
#1743=VECTOR('',#5602,0.4);
#1744=VECTOR('',#5607,0.425);
#1745=VECTOR('',#5612,0.41);
#1746=VECTOR('',#5621,0.26);
#1747=VECTOR('',#5626,0.25);
#1748=VECTOR('',#5631,0.225);
#1749=VECTOR('',#5636,1.);
#1750=VECTOR('',#5637,1.);
#1751=VECTOR('',#5638,1.);
#1752=VECTOR('',#5639,1.);
#1753=VECTOR('',#5642,1.);
#1754=VECTOR('',#5643,1.);
#1755=VECTOR('',#5644,1.);
#1756=VECTOR('',#5647,1.);
#1757=VECTOR('',#5648,1.);
#1758=VECTOR('',#5649,1.);
#1759=VECTOR('',#5652,1.);
#1760=VECTOR('',#5653,1.);
#1761=VECTOR('',#5654,1.);
#1762=VECTOR('',#5657,1.);
#1763=VECTOR('',#5658,1.);
#1764=VECTOR('',#5659,1.);
#1765=VECTOR('',#5662,1.);
#1766=VECTOR('',#5663,1.);
#1767=VECTOR('',#5674,0.265);
#1768=VECTOR('',#5681,0.5);
#1769=VECTOR('',#5692,0.47094010767585);
#1770=VECTOR('',#5699,0.47094010767585);
#1771=VECTOR('',#5702,1.);
#1772=VECTOR('',#5703,1.);
#1773=VECTOR('',#5706,1.);
#1774=VECTOR('',#5709,1.);
#1775=VECTOR('',#5714,0.25);
#1776=VECTOR('',#5719,1.);
#1777=VECTOR('',#5722,1.);
#1778=VECTOR('',#5783,0.225);
#1779=VECTOR('',#5790,0.225);
#1780=VECTOR('',#5797,0.449999999999999);
#1781=VECTOR('',#5804,0.449999999999999);
#1782=VECTOR('',#5809,1.);
#1783=VECTOR('',#5810,1.);
#1784=VECTOR('',#5811,1.);
#1785=VECTOR('',#5812,1.);
#1786=VECTOR('',#5815,1.);
#1787=VECTOR('',#5816,1.);
#1788=VECTOR('',#5817,1.);
#1789=VECTOR('',#5820,1.);
#1790=VECTOR('',#5821,1.);
#1791=VECTOR('',#5822,1.);
#1792=VECTOR('',#5825,1.);
#1793=VECTOR('',#5826,1.);
#1794=VECTOR('',#5837,0.164999999999999);
#1795=VECTOR('',#5846,0.164999999999999);
#1796=VECTOR('',#5853,1.);
#1797=VECTOR('',#5856,1.);
#1798=VECTOR('',#5861,1.);
#1799=VECTOR('',#5862,1.);
#1800=VECTOR('',#5863,1.);
#1801=VECTOR('',#5866,1.);
#1802=VECTOR('',#5867,1.);
#1803=VECTOR('',#5870,1.);
#1804=VECTOR('',#5871,1.);
#1805=VECTOR('',#5874,1.);
#1806=VECTOR('',#5883,0.4);
#1807=VECTOR('',#5896,0.4);
#1808=VECTOR('',#5907,1.);
#1809=VECTOR('',#5908,1.);
#1810=VECTOR('',#5909,1.);
#1811=VECTOR('',#5910,1.);
#1812=VECTOR('',#5913,1.);
#1813=VECTOR('',#5914,1.);
#1814=VECTOR('',#5915,1.);
#1815=VECTOR('',#5918,1.);
#1816=VECTOR('',#5919,1.);
#1817=VECTOR('',#5920,1.);
#1818=VECTOR('',#5923,1.);
#1819=VECTOR('',#5924,1.);
#1820=VECTOR('',#5925,1.);
#1821=VECTOR('',#5928,1.);
#1822=VECTOR('',#5929,1.);
#1823=VECTOR('',#5930,1.);
#1824=VECTOR('',#5933,1.);
#1825=VECTOR('',#5934,1.);
#1826=VECTOR('',#5951,0.325);
#1827=VECTOR('',#5956,0.35);
#1828=VECTOR('',#5961,0.335);
#1829=VECTOR('',#5970,0.21);
#1830=VECTOR('',#5973,0.2);
#1831=VECTOR('',#5980,0.42);
#1832=VECTOR('',#5987,0.8);
#1833=VECTOR('',#5998,0.734027674973257);
#1834=VECTOR('',#6005,0.734027674973257);
#1835=VECTOR('',#6008,1.);
#1836=VECTOR('',#6009,1.);
#1837=VECTOR('',#6012,1.);
#1838=VECTOR('',#6015,1.);
#1839=VECTOR('',#6020,0.4);
#1840=VECTOR('',#6025,1.);
#1841=VECTOR('',#6028,1.);
#1842=VECTOR('',#6071,1.5);
#1843=VERTEX_POINT('',#6090);
#1844=VERTEX_POINT('',#6091);
#1845=VERTEX_POINT('',#6093);
#1846=VERTEX_POINT('',#6095);
#1847=VERTEX_POINT('',#6099);
#1848=VERTEX_POINT('',#6101);
#1849=VERTEX_POINT('',#6105);
#1850=VERTEX_POINT('',#6107);
#1851=VERTEX_POINT('',#6115);
#1852=VERTEX_POINT('',#6116);
#1853=VERTEX_POINT('',#6118);
#1854=VERTEX_POINT('',#6120);
#1855=VERTEX_POINT('',#6124);
#1856=VERTEX_POINT('',#6126);
#1857=VERTEX_POINT('',#6130);
#1858=VERTEX_POINT('',#6132);
#1859=VERTEX_POINT('',#6140);
#1860=VERTEX_POINT('',#6142);
#1861=VERTEX_POINT('',#6146);
#1862=VERTEX_POINT('',#6148);
#1863=VERTEX_POINT('',#6152);
#1864=VERTEX_POINT('',#6154);
#1865=VERTEX_POINT('',#6158);
#1866=VERTEX_POINT('',#6160);
#1867=VERTEX_POINT('',#6164);
#1868=VERTEX_POINT('',#6166);
#1869=VERTEX_POINT('',#6170);
#1870=VERTEX_POINT('',#6172);
#1871=VERTEX_POINT('',#6176);
#1872=VERTEX_POINT('',#6178);
#1873=VERTEX_POINT('',#6182);
#1874=VERTEX_POINT('',#6184);
#1875=VERTEX_POINT('',#6188);
#1876=VERTEX_POINT('',#6190);
#1877=VERTEX_POINT('',#6194);
#1878=VERTEX_POINT('',#6196);
#1879=VERTEX_POINT('',#6200);
#1880=VERTEX_POINT('',#6202);
#1881=VERTEX_POINT('',#6206);
#1882=VERTEX_POINT('',#6208);
#1883=VERTEX_POINT('',#6212);
#1884=VERTEX_POINT('',#6213);
#1885=VERTEX_POINT('',#6215);
#1886=VERTEX_POINT('',#6217);
#1887=VERTEX_POINT('',#6221);
#1888=VERTEX_POINT('',#6223);
#1889=VERTEX_POINT('',#6227);
#1890=VERTEX_POINT('',#6229);
#1891=VERTEX_POINT('',#6239);
#1892=VERTEX_POINT('',#6241);
#1893=VERTEX_POINT('',#6245);
#1894=VERTEX_POINT('',#6247);
#1895=VERTEX_POINT('',#6251);
#1896=VERTEX_POINT('',#6252);
#1897=VERTEX_POINT('',#6254);
#1898=VERTEX_POINT('',#6256);
#1899=VERTEX_POINT('',#6260);
#1900=VERTEX_POINT('',#6262);
#1901=VERTEX_POINT('',#6266);
#1902=VERTEX_POINT('',#6268);
#1903=VERTEX_POINT('',#6278);
#1904=VERTEX_POINT('',#6279);
#1905=VERTEX_POINT('',#6281);
#1906=VERTEX_POINT('',#6283);
#1907=VERTEX_POINT('',#6287);
#1908=VERTEX_POINT('',#6289);
#1909=VERTEX_POINT('',#6293);
#1910=VERTEX_POINT('',#6295);
#1911=VERTEX_POINT('',#6305);
#1912=VERTEX_POINT('',#6307);
#1913=VERTEX_POINT('',#6311);
#1914=VERTEX_POINT('',#6313);
#1915=VERTEX_POINT('',#6317);
#1916=VERTEX_POINT('',#6318);
#1917=VERTEX_POINT('',#6320);
#1918=VERTEX_POINT('',#6322);
#1919=VERTEX_POINT('',#6326);
#1920=VERTEX_POINT('',#6328);
#1921=VERTEX_POINT('',#6332);
#1922=VERTEX_POINT('',#6334);
#1923=VERTEX_POINT('',#6344);
#1924=VERTEX_POINT('',#6345);
#1925=VERTEX_POINT('',#6347);
#1926=VERTEX_POINT('',#6349);
#1927=VERTEX_POINT('',#6353);
#1928=VERTEX_POINT('',#6355);
#1929=VERTEX_POINT('',#6359);
#1930=VERTEX_POINT('',#6361);
#1931=VERTEX_POINT('',#6371);
#1932=VERTEX_POINT('',#6372);
#1933=VERTEX_POINT('',#6374);
#1934=VERTEX_POINT('',#6376);
#1935=VERTEX_POINT('',#6380);
#1936=VERTEX_POINT('',#6381);
#1937=VERTEX_POINT('',#6383);
#1938=VERTEX_POINT('',#6385);
#1939=VERTEX_POINT('',#6387);
#1940=VERTEX_POINT('',#6391);
#1941=VERTEX_POINT('',#6392);
#1942=VERTEX_POINT('',#6394);
#1943=VERTEX_POINT('',#6396);
#1944=VERTEX_POINT('',#6400);
#1945=VERTEX_POINT('',#6402);
#1946=VERTEX_POINT('',#6406);
#1947=VERTEX_POINT('',#6408);
#1948=VERTEX_POINT('',#6420);
#1949=VERTEX_POINT('',#6423);
#1950=VERTEX_POINT('',#6429);
#1951=VERTEX_POINT('',#6432);
#1952=VERTEX_POINT('',#6434);
#1953=VERTEX_POINT('',#6436);
#1954=VERTEX_POINT('',#6438);
#1955=VERTEX_POINT('',#6442);
#1956=VERTEX_POINT('',#6446);
#1957=VERTEX_POINT('',#6449);
#1958=VERTEX_POINT('',#6453);
#1959=VERTEX_POINT('',#6457);
#1960=VERTEX_POINT('',#6461);
#1961=VERTEX_POINT('',#6465);
#1962=VERTEX_POINT('',#6469);
#1963=VERTEX_POINT('',#6473);
#1964=VERTEX_POINT('',#6475);
#1965=VERTEX_POINT('',#6479);
#1966=VERTEX_POINT('',#6483);
#1967=VERTEX_POINT('',#6491);
#1968=VERTEX_POINT('',#6492);
#1969=VERTEX_POINT('',#6494);
#1970=VERTEX_POINT('',#6496);
#1971=VERTEX_POINT('',#6500);
#1972=VERTEX_POINT('',#6501);
#1973=VERTEX_POINT('',#6503);
#1974=VERTEX_POINT('',#6505);
#1975=VERTEX_POINT('',#6507);
#1976=VERTEX_POINT('',#6511);
#1977=VERTEX_POINT('',#6512);
#1978=VERTEX_POINT('',#6514);
#1979=VERTEX_POINT('',#6516);
#1980=VERTEX_POINT('',#6520);
#1981=VERTEX_POINT('',#6522);
#1982=VERTEX_POINT('',#6526);
#1983=VERTEX_POINT('',#6528);
#1984=VERTEX_POINT('',#6540);
#1985=VERTEX_POINT('',#6543);
#1986=VERTEX_POINT('',#6549);
#1987=VERTEX_POINT('',#6552);
#1988=VERTEX_POINT('',#6554);
#1989=VERTEX_POINT('',#6556);
#1990=VERTEX_POINT('',#6558);
#1991=VERTEX_POINT('',#6562);
#1992=VERTEX_POINT('',#6566);
#1993=VERTEX_POINT('',#6569);
#1994=VERTEX_POINT('',#6573);
#1995=VERTEX_POINT('',#6577);
#1996=VERTEX_POINT('',#6581);
#1997=VERTEX_POINT('',#6585);
#1998=VERTEX_POINT('',#6589);
#1999=VERTEX_POINT('',#6593);
#2000=VERTEX_POINT('',#6595);
#2001=VERTEX_POINT('',#6599);
#2002=VERTEX_POINT('',#6603);
#2003=VERTEX_POINT('',#6611);
#2004=VERTEX_POINT('',#6613);
#2005=VERTEX_POINT('',#6617);
#2006=VERTEX_POINT('',#6618);
#2007=VERTEX_POINT('',#6620);
#2008=VERTEX_POINT('',#6622);
#2009=VERTEX_POINT('',#6631);
#2010=VERTEX_POINT('',#6634);
#2011=VERTEX_POINT('',#6635);
#2012=VERTEX_POINT('',#6637);
#2013=VERTEX_POINT('',#6639);
#2014=VERTEX_POINT('',#6648);
#2015=VERTEX_POINT('',#6651);
#2016=VERTEX_POINT('',#6653);
#2017=VERTEX_POINT('',#6660);
#2018=VERTEX_POINT('',#6662);
#2019=VERTEX_POINT('',#6666);
#2020=VERTEX_POINT('',#6670);
#2021=VERTEX_POINT('',#6674);
#2022=VERTEX_POINT('',#6675);
#2023=VERTEX_POINT('',#6680);
#2024=VERTEX_POINT('',#6684);
#2025=VERTEX_POINT('',#6692);
#2026=VERTEX_POINT('',#6693);
#2027=VERTEX_POINT('',#6695);
#2028=VERTEX_POINT('',#6697);
#2029=VERTEX_POINT('',#6699);
#2030=VERTEX_POINT('',#6701);
#2031=VERTEX_POINT('',#6703);
#2032=VERTEX_POINT('',#6705);
#2033=VERTEX_POINT('',#6709);
#2034=VERTEX_POINT('',#6711);
#2035=VERTEX_POINT('',#6715);
#2036=VERTEX_POINT('',#6719);
#2037=VERTEX_POINT('',#6723);
#2038=VERTEX_POINT('',#6727);
#2039=VERTEX_POINT('',#6728);
#2040=VERTEX_POINT('',#6731);
#2041=VERTEX_POINT('',#6743);
#2042=VERTEX_POINT('',#6746);
#2043=VERTEX_POINT('',#6750);
#2044=VERTEX_POINT('',#6754);
#2045=VERTEX_POINT('',#6758);
#2046=VERTEX_POINT('',#6761);
#2047=VERTEX_POINT('',#6765);
#2048=VERTEX_POINT('',#6769);
#2049=VERTEX_POINT('',#6774);
#2050=VERTEX_POINT('',#6775);
#2051=VERTEX_POINT('',#6777);
#2052=VERTEX_POINT('',#6779);
#2053=VERTEX_POINT('',#6783);
#2054=VERTEX_POINT('',#6785);
#2055=VERTEX_POINT('',#6789);
#2056=VERTEX_POINT('',#6791);
#2057=VERTEX_POINT('',#6795);
#2058=VERTEX_POINT('',#6797);
#2059=VERTEX_POINT('',#6801);
#2060=VERTEX_POINT('',#6803);
#2061=VERTEX_POINT('',#6813);
#2062=VERTEX_POINT('',#6816);
#2063=VERTEX_POINT('',#6820);
#2064=VERTEX_POINT('',#6824);
#2065=VERTEX_POINT('',#6828);
#2066=VERTEX_POINT('',#6831);
#2067=VERTEX_POINT('',#6835);
#2068=VERTEX_POINT('',#6839);
#2069=VERTEX_POINT('',#6844);
#2070=VERTEX_POINT('',#6845);
#2071=VERTEX_POINT('',#6847);
#2072=VERTEX_POINT('',#6849);
#2073=VERTEX_POINT('',#6853);
#2074=VERTEX_POINT('',#6855);
#2075=VERTEX_POINT('',#6859);
#2076=VERTEX_POINT('',#6861);
#2077=VERTEX_POINT('',#6865);
#2078=VERTEX_POINT('',#6867);
#2079=VERTEX_POINT('',#6871);
#2080=VERTEX_POINT('',#6873);
#2081=VERTEX_POINT('',#6883);
#2082=VERTEX_POINT('',#6885);
#2083=VERTEX_POINT('',#6889);
#2084=VERTEX_POINT('',#6891);
#2085=VERTEX_POINT('',#6898);
#2086=VERTEX_POINT('',#6899);
#2087=VERTEX_POINT('',#6903);
#2088=VERTEX_POINT('',#6907);
#2089=VERTEX_POINT('',#6910);
#2090=VERTEX_POINT('',#6914);
#2091=VERTEX_POINT('',#6918);
#2092=VERTEX_POINT('',#6926);
#2093=VERTEX_POINT('',#6928);
#2094=VERTEX_POINT('',#6930);
#2095=VERTEX_POINT('',#6934);
#2096=VERTEX_POINT('',#6938);
#2097=VERTEX_POINT('',#6942);
#2098=VERTEX_POINT('',#6946);
#2099=VERTEX_POINT('',#6961);
#2100=VERTEX_POINT('',#6963);
#2101=VERTEX_POINT('',#6999);
#2102=VERTEX_POINT('',#7001);
#2103=VERTEX_POINT('',#7005);
#2104=VERTEX_POINT('',#7007);
#2105=VERTEX_POINT('',#7011);
#2106=VERTEX_POINT('',#7013);
#2107=VERTEX_POINT('',#7017);
#2108=VERTEX_POINT('',#7019);
#2109=VERTEX_POINT('',#7023);
#2110=VERTEX_POINT('',#7024);
#2111=VERTEX_POINT('',#7026);
#2112=VERTEX_POINT('',#7028);
#2113=VERTEX_POINT('',#7032);
#2114=VERTEX_POINT('',#7034);
#2115=VERTEX_POINT('',#7038);
#2116=VERTEX_POINT('',#7040);
#2117=VERTEX_POINT('',#7050);
#2118=VERTEX_POINT('',#7052);
#2119=VERTEX_POINT('',#7057);
#2120=VERTEX_POINT('',#7059);
#2121=VERTEX_POINT('',#7064);
#2122=VERTEX_POINT('',#7065);
#2123=VERTEX_POINT('',#7067);
#2124=VERTEX_POINT('',#7069);
#2125=VERTEX_POINT('',#7073);
#2126=VERTEX_POINT('',#7075);
#2127=VERTEX_POINT('',#7079);
#2128=VERTEX_POINT('',#7083);
#2129=VERTEX_POINT('',#7091);
#2130=VERTEX_POINT('',#7093);
#2131=VERTEX_POINT('',#7100);
#2132=VERTEX_POINT('',#7102);
#2133=VERTEX_POINT('',#7109);
#2134=VERTEX_POINT('',#7110);
#2135=VERTEX_POINT('',#7112);
#2136=VERTEX_POINT('',#7114);
#2137=VERTEX_POINT('',#7118);
#2138=VERTEX_POINT('',#7120);
#2139=VERTEX_POINT('',#7124);
#2140=VERTEX_POINT('',#7126);
#2141=VERTEX_POINT('',#7130);
#2142=VERTEX_POINT('',#7132);
#2143=VERTEX_POINT('',#7136);
#2144=VERTEX_POINT('',#7138);
#2145=VERTEX_POINT('',#7147);
#2146=VERTEX_POINT('',#7150);
#2147=VERTEX_POINT('',#7153);
#2148=VERTEX_POINT('',#7157);
#2149=VERTEX_POINT('',#7161);
#2150=VERTEX_POINT('',#7165);
#2151=VERTEX_POINT('',#7168);
#2152=VERTEX_POINT('',#7175);
#2153=VERTEX_POINT('',#7177);
#2154=VERTEX_POINT('',#7181);
#2155=VERTEX_POINT('',#7183);
#2156=VERTEX_POINT('',#7190);
#2157=VERTEX_POINT('',#7191);
#2158=VERTEX_POINT('',#7195);
#2159=VERTEX_POINT('',#7199);
#2160=VERTEX_POINT('',#7202);
#2161=VERTEX_POINT('',#7206);
#2162=VERTEX_POINT('',#7210);
#2163=VERTEX_POINT('',#7218);
#2164=VERTEX_POINT('',#7220);
#2165=VERTEX_POINT('',#7222);
#2166=VERTEX_POINT('',#7226);
#2167=VERTEX_POINT('',#7230);
#2168=VERTEX_POINT('',#7234);
#2169=VERTEX_POINT('',#7238);
#2170=VERTEX_POINT('',#7253);
#2171=VERTEX_POINT('',#7255);
#2172=VERTEX_POINT('',#7282);
#2173=VERTEX_POINT('',#7284);
#2174=EDGE_CURVE('',#1843,#1844,#1113,.T.);
#2175=EDGE_CURVE('',#1845,#1843,#1114,.T.);
#2176=EDGE_CURVE('',#1846,#1845,#1115,.T.);
#2177=EDGE_CURVE('',#1846,#1844,#1116,.T.);
#2178=EDGE_CURVE('',#1844,#1847,#1117,.T.);
#2179=EDGE_CURVE('',#1848,#1846,#1118,.T.);
#2180=EDGE_CURVE('',#1848,#1847,#1119,.T.);
#2181=EDGE_CURVE('',#1847,#1849,#1120,.T.);
#2182=EDGE_CURVE('',#1850,#1848,#1121,.T.);
#2183=EDGE_CURVE('',#1850,#1849,#1122,.T.);
#2184=EDGE_CURVE('',#1849,#1843,#1123,.T.);
#2185=EDGE_CURVE('',#1845,#1850,#1124,.T.);
#2186=EDGE_CURVE('',#1851,#1852,#1125,.T.);
#2187=EDGE_CURVE('',#1853,#1851,#1126,.T.);
#2188=EDGE_CURVE('',#1854,#1853,#1127,.T.);
#2189=EDGE_CURVE('',#1854,#1852,#1128,.T.);
#2190=EDGE_CURVE('',#1852,#1855,#1129,.T.);
#2191=EDGE_CURVE('',#1856,#1854,#1130,.T.);
#2192=EDGE_CURVE('',#1856,#1855,#1131,.T.);
#2193=EDGE_CURVE('',#1855,#1857,#1132,.T.);
#2194=EDGE_CURVE('',#1858,#1856,#1133,.T.);
#2195=EDGE_CURVE('',#1858,#1857,#1134,.T.);
#2196=EDGE_CURVE('',#1857,#1851,#1135,.T.);
#2197=EDGE_CURVE('',#1853,#1858,#1136,.T.);
#2198=EDGE_CURVE('',#1859,#1859,#376,.T.);
#2199=EDGE_CURVE('',#1859,#1860,#1137,.T.);
#2200=EDGE_CURVE('',#1860,#1860,#377,.T.);
#2201=EDGE_CURVE('',#1861,#1861,#378,.T.);
#2202=EDGE_CURVE('',#1861,#1862,#1138,.T.);
#2203=EDGE_CURVE('',#1862,#1862,#379,.T.);
#2204=EDGE_CURVE('',#1863,#1863,#380,.T.);
#2205=EDGE_CURVE('',#1863,#1864,#1139,.T.);
#2206=EDGE_CURVE('',#1864,#1864,#381,.T.);
#2207=EDGE_CURVE('',#1865,#1865,#382,.T.);
#2208=EDGE_CURVE('',#1865,#1866,#1140,.T.);
#2209=EDGE_CURVE('',#1866,#1866,#383,.T.);
#2210=EDGE_CURVE('',#1867,#1867,#384,.T.);
#2211=EDGE_CURVE('',#1867,#1868,#1141,.T.);
#2212=EDGE_CURVE('',#1868,#1868,#385,.T.);
#2213=EDGE_CURVE('',#1869,#1869,#386,.T.);
#2214=EDGE_CURVE('',#1869,#1870,#1142,.T.);
#2215=EDGE_CURVE('',#1870,#1870,#387,.T.);
#2216=EDGE_CURVE('',#1871,#1871,#388,.T.);
#2217=EDGE_CURVE('',#1871,#1872,#1143,.T.);
#2218=EDGE_CURVE('',#1872,#1872,#389,.T.);
#2219=EDGE_CURVE('',#1873,#1873,#390,.T.);
#2220=EDGE_CURVE('',#1873,#1874,#1144,.T.);
#2221=EDGE_CURVE('',#1874,#1874,#391,.T.);
#2222=EDGE_CURVE('',#1875,#1875,#392,.T.);
#2223=EDGE_CURVE('',#1875,#1876,#1145,.T.);
#2224=EDGE_CURVE('',#1876,#1876,#393,.T.);
#2225=EDGE_CURVE('',#1877,#1877,#394,.T.);
#2226=EDGE_CURVE('',#1877,#1878,#1146,.T.);
#2227=EDGE_CURVE('',#1878,#1878,#395,.T.);
#2228=EDGE_CURVE('',#1879,#1879,#396,.T.);
#2229=EDGE_CURVE('',#1879,#1880,#1147,.T.);
#2230=EDGE_CURVE('',#1880,#1880,#397,.T.);
#2231=EDGE_CURVE('',#1881,#1881,#398,.T.);
#2232=EDGE_CURVE('',#1881,#1882,#1148,.T.);
#2233=EDGE_CURVE('',#1882,#1882,#399,.T.);
#2234=EDGE_CURVE('',#1883,#1884,#1149,.T.);
#2235=EDGE_CURVE('',#1884,#1885,#1150,.T.);
#2236=EDGE_CURVE('',#1886,#1885,#1151,.T.);
#2237=EDGE_CURVE('',#1883,#1886,#1152,.T.);
#2238=EDGE_CURVE('',#1887,#1883,#1153,.T.);
#2239=EDGE_CURVE('',#1888,#1886,#1154,.T.);
#2240=EDGE_CURVE('',#1887,#1888,#1155,.T.);
#2241=EDGE_CURVE('',#1889,#1887,#1156,.T.);
#2242=EDGE_CURVE('',#1890,#1888,#1157,.T.);
#2243=EDGE_CURVE('',#1889,#1890,#1158,.T.);
#2244=EDGE_CURVE('',#1884,#1889,#1159,.T.);
#2245=EDGE_CURVE('',#1885,#1890,#1160,.T.);
#2246=EDGE_CURVE('',#1891,#1891,#400,.T.);
#2247=EDGE_CURVE('',#1891,#1892,#1161,.T.);
#2248=EDGE_CURVE('',#1892,#1892,#401,.T.);
#2249=EDGE_CURVE('',#1893,#1893,#402,.T.);
#2250=EDGE_CURVE('',#1893,#1894,#1162,.T.);
#2251=EDGE_CURVE('',#1894,#1894,#403,.T.);
#2252=EDGE_CURVE('',#1895,#1896,#1163,.T.);
#2253=EDGE_CURVE('',#1896,#1897,#1164,.T.);
#2254=EDGE_CURVE('',#1898,#1897,#1165,.T.);
#2255=EDGE_CURVE('',#1895,#1898,#1166,.T.);
#2256=EDGE_CURVE('',#1899,#1895,#1167,.T.);
#2257=EDGE_CURVE('',#1900,#1898,#1168,.T.);
#2258=EDGE_CURVE('',#1899,#1900,#1169,.T.);
#2259=EDGE_CURVE('',#1901,#1899,#1170,.T.);
#2260=EDGE_CURVE('',#1902,#1900,#1171,.T.);
#2261=EDGE_CURVE('',#1901,#1902,#1172,.T.);
#2262=EDGE_CURVE('',#1896,#1901,#1173,.T.);
#2263=EDGE_CURVE('',#1897,#1902,#1174,.T.);
#2264=EDGE_CURVE('',#1903,#1904,#1175,.T.);
#2265=EDGE_CURVE('',#1904,#1905,#1176,.T.);
#2266=EDGE_CURVE('',#1906,#1905,#1177,.T.);
#2267=EDGE_CURVE('',#1903,#1906,#1178,.T.);
#2268=EDGE_CURVE('',#1907,#1903,#1179,.T.);
#2269=EDGE_CURVE('',#1908,#1906,#1180,.T.);
#2270=EDGE_CURVE('',#1907,#1908,#1181,.T.);
#2271=EDGE_CURVE('',#1909,#1907,#1182,.T.);
#2272=EDGE_CURVE('',#1910,#1908,#1183,.T.);
#2273=EDGE_CURVE('',#1909,#1910,#1184,.T.);
#2274=EDGE_CURVE('',#1904,#1909,#1185,.T.);
#2275=EDGE_CURVE('',#1905,#1910,#1186,.T.);
#2276=EDGE_CURVE('',#1911,#1911,#404,.T.);
#2277=EDGE_CURVE('',#1911,#1912,#1187,.T.);
#2278=EDGE_CURVE('',#1912,#1912,#405,.T.);
#2279=EDGE_CURVE('',#1913,#1913,#406,.T.);
#2280=EDGE_CURVE('',#1913,#1914,#1188,.T.);
#2281=EDGE_CURVE('',#1914,#1914,#407,.T.);
#2282=EDGE_CURVE('',#1915,#1916,#1189,.T.);
#2283=EDGE_CURVE('',#1916,#1917,#1190,.T.);
#2284=EDGE_CURVE('',#1918,#1917,#1191,.T.);
#2285=EDGE_CURVE('',#1915,#1918,#1192,.T.);
#2286=EDGE_CURVE('',#1919,#1915,#1193,.T.);
#2287=EDGE_CURVE('',#1920,#1918,#1194,.T.);
#2288=EDGE_CURVE('',#1919,#1920,#1195,.T.);
#2289=EDGE_CURVE('',#1921,#1919,#1196,.T.);
#2290=EDGE_CURVE('',#1922,#1920,#1197,.T.);
#2291=EDGE_CURVE('',#1921,#1922,#1198,.T.);
#2292=EDGE_CURVE('',#1916,#1921,#1199,.T.);
#2293=EDGE_CURVE('',#1917,#1922,#1200,.T.);
#2294=EDGE_CURVE('',#1923,#1924,#1201,.T.);
#2295=EDGE_CURVE('',#1924,#1925,#1202,.T.);
#2296=EDGE_CURVE('',#1926,#1925,#1203,.T.);
#2297=EDGE_CURVE('',#1923,#1926,#1204,.T.);
#2298=EDGE_CURVE('',#1927,#1923,#1205,.T.);
#2299=EDGE_CURVE('',#1928,#1926,#1206,.T.);
#2300=EDGE_CURVE('',#1927,#1928,#1207,.T.);
#2301=EDGE_CURVE('',#1929,#1927,#1208,.T.);
#2302=EDGE_CURVE('',#1930,#1928,#1209,.T.);
#2303=EDGE_CURVE('',#1929,#1930,#1210,.T.);
#2304=EDGE_CURVE('',#1924,#1929,#1211,.T.);
#2305=EDGE_CURVE('',#1925,#1930,#1212,.T.);
#2306=EDGE_CURVE('',#1931,#1932,#1213,.T.);
#2307=EDGE_CURVE('',#1933,#1931,#408,.T.);
#2308=EDGE_CURVE('',#1933,#1934,#1214,.T.);
#2309=EDGE_CURVE('',#1932,#1934,#409,.T.);
#2310=EDGE_CURVE('',#1935,#1936,#1215,.T.);
#2311=EDGE_CURVE('',#1937,#1935,#410,.T.);
#2312=EDGE_CURVE('',#1937,#1938,#1216,.T.);
#2313=EDGE_CURVE('',#1939,#1938,#411,.T.);
#2314=EDGE_CURVE('',#1936,#1939,#220,.T.);
#2315=EDGE_CURVE('',#1940,#1941,#1217,.T.);
#2316=EDGE_CURVE('',#1940,#1942,#1218,.T.);
#2317=EDGE_CURVE('',#1942,#1943,#1219,.T.);
#2318=EDGE_CURVE('',#1941,#1943,#1220,.T.);
#2319=EDGE_CURVE('',#1941,#1944,#1221,.T.);
#2320=EDGE_CURVE('',#1943,#1945,#1222,.T.);
#2321=EDGE_CURVE('',#1944,#1945,#1223,.T.);
#2322=EDGE_CURVE('',#1944,#1946,#1224,.T.);
#2323=EDGE_CURVE('',#1945,#1947,#1225,.T.);
#2324=EDGE_CURVE('',#1946,#1947,#1226,.T.);
#2325=EDGE_CURVE('',#1946,#1940,#1227,.T.);
#2326=EDGE_CURVE('',#1947,#1942,#1228,.T.);
#2327=EDGE_CURVE('',#1938,#1936,#412,.T.);
#2328=EDGE_CURVE('',#1937,#1938,#1229,.T.);
#2329=EDGE_CURVE('',#1935,#1937,#413,.T.);
#2330=EDGE_CURVE('',#1948,#1948,#414,.T.);
#2331=EDGE_CURVE('',#1949,#1932,#221,.T.);
#2332=EDGE_CURVE('',#1934,#1949,#415,.T.);
#2333=EDGE_CURVE('',#1933,#1934,#1230,.T.);
#2334=EDGE_CURVE('',#1931,#1933,#416,.T.);
#2335=EDGE_CURVE('',#1950,#1950,#417,.T.);
#2336=EDGE_CURVE('',#1951,#1939,#1231,.T.);
#2337=EDGE_CURVE('',#1952,#1951,#1232,.T.);
#2338=EDGE_CURVE('',#1953,#1952,#1233,.T.);
#2339=EDGE_CURVE('',#1954,#1953,#1234,.T.);
#2340=EDGE_CURVE('',#1936,#1954,#1235,.T.);
#2341=EDGE_CURVE('',#1938,#1955,#1236,.T.);
#2342=EDGE_CURVE('',#1955,#1951,#1237,.T.);
#2343=EDGE_CURVE('',#1956,#1932,#1238,.T.);
#2344=EDGE_CURVE('',#1953,#1956,#1239,.T.);
#2345=EDGE_CURVE('',#1957,#1952,#1240,.T.);
#2346=EDGE_CURVE('',#1949,#1957,#1241,.T.);
#2347=EDGE_CURVE('',#1934,#1958,#1242,.T.);
#2348=EDGE_CURVE('',#1958,#1956,#1243,.T.);
#2349=EDGE_CURVE('',#1959,#1959,#418,.T.);
#2350=EDGE_CURVE('',#1959,#1948,#1244,.T.);
#2351=EDGE_CURVE('',#1960,#1960,#419,.T.);
#2352=EDGE_CURVE('',#1960,#1950,#1245,.T.);
#2353=EDGE_CURVE('',#1954,#1961,#1246,.T.);
#2354=EDGE_CURVE('',#1961,#1938,#1247,.T.);
#2355=EDGE_CURVE('',#1957,#1962,#1248,.T.);
#2356=EDGE_CURVE('',#1962,#1934,#1249,.T.);
#2357=EDGE_CURVE('',#1963,#1958,#1250,.T.);
#2358=EDGE_CURVE('',#1963,#1964,#1251,.T.);
#2359=EDGE_CURVE('',#1964,#1961,#1252,.T.);
#2360=EDGE_CURVE('',#1965,#1963,#1253,.T.);
#2361=EDGE_CURVE('',#1965,#1962,#1254,.T.);
#2362=EDGE_CURVE('',#1966,#1955,#1255,.T.);
#2363=EDGE_CURVE('',#1966,#1965,#1256,.T.);
#2364=EDGE_CURVE('',#1964,#1966,#1257,.T.);
#2365=EDGE_CURVE('',#1967,#1968,#1258,.T.);
#2366=EDGE_CURVE('',#1969,#1967,#420,.T.);
#2367=EDGE_CURVE('',#1969,#1970,#1259,.T.);
#2368=EDGE_CURVE('',#1968,#1970,#421,.T.);
#2369=EDGE_CURVE('',#1971,#1972,#1260,.T.);
#2370=EDGE_CURVE('',#1973,#1971,#422,.T.);
#2371=EDGE_CURVE('',#1973,#1974,#1261,.T.);
#2372=EDGE_CURVE('',#1975,#1974,#423,.T.);
#2373=EDGE_CURVE('',#1972,#1975,#222,.T.);
#2374=EDGE_CURVE('',#1976,#1977,#1262,.T.);
#2375=EDGE_CURVE('',#1976,#1978,#1263,.T.);
#2376=EDGE_CURVE('',#1978,#1979,#1264,.T.);
#2377=EDGE_CURVE('',#1977,#1979,#1265,.T.);
#2378=EDGE_CURVE('',#1977,#1980,#1266,.T.);
#2379=EDGE_CURVE('',#1979,#1981,#1267,.T.);
#2380=EDGE_CURVE('',#1980,#1981,#1268,.T.);
#2381=EDGE_CURVE('',#1980,#1982,#1269,.T.);
#2382=EDGE_CURVE('',#1981,#1983,#1270,.T.);
#2383=EDGE_CURVE('',#1982,#1983,#1271,.T.);
#2384=EDGE_CURVE('',#1982,#1976,#1272,.T.);
#2385=EDGE_CURVE('',#1983,#1978,#1273,.T.);
#2386=EDGE_CURVE('',#1974,#1972,#424,.T.);
#2387=EDGE_CURVE('',#1973,#1974,#1274,.T.);
#2388=EDGE_CURVE('',#1971,#1973,#425,.T.);
#2389=EDGE_CURVE('',#1984,#1984,#426,.T.);
#2390=EDGE_CURVE('',#1985,#1968,#223,.T.);
#2391=EDGE_CURVE('',#1970,#1985,#427,.T.);
#2392=EDGE_CURVE('',#1969,#1970,#1275,.T.);
#2393=EDGE_CURVE('',#1967,#1969,#428,.T.);
#2394=EDGE_CURVE('',#1986,#1986,#429,.T.);
#2395=EDGE_CURVE('',#1987,#1975,#1276,.T.);
#2396=EDGE_CURVE('',#1988,#1987,#1277,.T.);
#2397=EDGE_CURVE('',#1989,#1988,#1278,.T.);
#2398=EDGE_CURVE('',#1990,#1989,#1279,.T.);
#2399=EDGE_CURVE('',#1972,#1990,#1280,.T.);
#2400=EDGE_CURVE('',#1974,#1991,#1281,.T.);
#2401=EDGE_CURVE('',#1991,#1987,#1282,.T.);
#2402=EDGE_CURVE('',#1992,#1968,#1283,.T.);
#2403=EDGE_CURVE('',#1989,#1992,#1284,.T.);
#2404=EDGE_CURVE('',#1993,#1988,#1285,.T.);
#2405=EDGE_CURVE('',#1985,#1993,#1286,.T.);
#2406=EDGE_CURVE('',#1970,#1994,#1287,.T.);
#2407=EDGE_CURVE('',#1994,#1992,#1288,.T.);
#2408=EDGE_CURVE('',#1995,#1995,#430,.T.);
#2409=EDGE_CURVE('',#1995,#1984,#1289,.T.);
#2410=EDGE_CURVE('',#1996,#1996,#431,.T.);
#2411=EDGE_CURVE('',#1996,#1986,#1290,.T.);
#2412=EDGE_CURVE('',#1990,#1997,#1291,.T.);
#2413=EDGE_CURVE('',#1997,#1974,#1292,.T.);
#2414=EDGE_CURVE('',#1993,#1998,#1293,.T.);
#2415=EDGE_CURVE('',#1998,#1970,#1294,.T.);
#2416=EDGE_CURVE('',#1999,#1994,#1295,.T.);
#2417=EDGE_CURVE('',#1999,#2000,#1296,.T.);
#2418=EDGE_CURVE('',#2000,#1997,#1297,.T.);
#2419=EDGE_CURVE('',#2001,#1999,#1298,.T.);
#2420=EDGE_CURVE('',#2001,#1998,#1299,.T.);
#2421=EDGE_CURVE('',#2002,#1991,#1300,.T.);
#2422=EDGE_CURVE('',#2002,#2001,#1301,.T.);
#2423=EDGE_CURVE('',#2000,#2002,#1302,.T.);
#2424=EDGE_CURVE('',#2003,#2003,#432,.T.);
#2425=EDGE_CURVE('',#2003,#2004,#1303,.T.);
#2426=EDGE_CURVE('',#2004,#2004,#433,.T.);
#2427=EDGE_CURVE('',#2005,#2006,#1304,.T.);
#2428=EDGE_CURVE('',#2007,#2006,#434,.T.);
#2429=EDGE_CURVE('',#2008,#2007,#1305,.T.);
#2430=EDGE_CURVE('',#2005,#2008,#435,.T.);
#2431=EDGE_CURVE('',#2005,#2006,#1306,.T.);
#2432=EDGE_CURVE('',#2008,#2005,#436,.T.);
#2433=EDGE_CURVE('',#2008,#2007,#1307,.T.);
#2434=EDGE_CURVE('',#2006,#2007,#437,.T.);
#2435=EDGE_CURVE('',#2009,#2009,#438,.T.);
#2436=EDGE_CURVE('',#2010,#2011,#1308,.T.);
#2437=EDGE_CURVE('',#2012,#2011,#439,.T.);
#2438=EDGE_CURVE('',#2013,#2012,#1309,.T.);
#2439=EDGE_CURVE('',#2010,#2013,#440,.T.);
#2440=EDGE_CURVE('',#2010,#2011,#1310,.T.);
#2441=EDGE_CURVE('',#2013,#2010,#441,.T.);
#2442=EDGE_CURVE('',#2013,#2012,#1311,.T.);
#2443=EDGE_CURVE('',#2011,#2012,#442,.T.);
#2444=EDGE_CURVE('',#2014,#2014,#443,.T.);
#2445=EDGE_CURVE('',#2011,#2015,#1312,.T.);
#2446=EDGE_CURVE('',#2015,#2016,#1313,.T.);
#2447=EDGE_CURVE('',#2016,#2012,#1314,.T.);
#2448=EDGE_CURVE('',#2006,#2011,#1315,.T.);
#2449=EDGE_CURVE('',#2012,#2007,#1316,.T.);
#2450=EDGE_CURVE('',#2007,#2017,#1317,.T.);
#2451=EDGE_CURVE('',#2017,#2018,#1318,.T.);
#2452=EDGE_CURVE('',#2018,#2006,#1319,.T.);
#2453=EDGE_CURVE('',#2019,#2019,#444,.T.);
#2454=EDGE_CURVE('',#2019,#2009,#1320,.T.);
#2455=EDGE_CURVE('',#2020,#2020,#445,.T.);
#2456=EDGE_CURVE('',#2020,#2014,#1321,.T.);
#2457=EDGE_CURVE('',#2021,#2022,#1322,.T.);
#2458=EDGE_CURVE('',#2022,#2016,#1323,.T.);
#2459=EDGE_CURVE('',#2021,#2015,#1324,.T.);
#2460=EDGE_CURVE('',#2023,#2021,#1325,.T.);
#2461=EDGE_CURVE('',#2023,#2018,#1326,.T.);
#2462=EDGE_CURVE('',#2024,#2023,#1327,.T.);
#2463=EDGE_CURVE('',#2024,#2017,#1328,.T.);
#2464=EDGE_CURVE('',#2022,#2024,#1329,.T.);
#2465=EDGE_CURVE('',#2025,#2026,#1330,.T.);
#2466=EDGE_CURVE('',#2027,#2025,#1331,.T.);
#2467=EDGE_CURVE('',#2028,#2027,#1332,.T.);
#2468=EDGE_CURVE('',#2029,#2028,#1333,.T.);
#2469=EDGE_CURVE('',#2030,#2029,#1334,.T.);
#2470=EDGE_CURVE('',#2031,#2030,#1335,.T.);
#2471=EDGE_CURVE('',#2032,#2031,#1336,.T.);
#2472=EDGE_CURVE('',#2026,#2032,#1337,.T.);
#2473=EDGE_CURVE('',#2029,#2033,#1338,.T.);
#2474=EDGE_CURVE('',#2033,#2034,#1339,.T.);
#2475=EDGE_CURVE('',#2034,#2030,#1340,.T.);
#2476=EDGE_CURVE('',#2035,#2028,#1341,.T.);
#2477=EDGE_CURVE('',#2035,#2033,#1342,.T.);
#2478=EDGE_CURVE('',#2027,#2036,#1343,.T.);
#2479=EDGE_CURVE('',#2036,#2035,#1344,.T.);
#2480=EDGE_CURVE('',#2037,#2025,#1345,.T.);
#2481=EDGE_CURVE('',#2037,#2036,#1346,.T.);
#2482=EDGE_CURVE('',#2038,#2039,#1347,.T.);
#2483=EDGE_CURVE('',#2034,#2038,#1348,.T.);
#2484=EDGE_CURVE('',#2040,#2037,#1349,.T.);
#2485=EDGE_CURVE('',#2039,#2040,#1350,.T.);
#2486=EDGE_CURVE('',#2031,#2038,#1351,.T.);
#2487=EDGE_CURVE('',#2026,#2040,#1352,.T.);
#2488=EDGE_CURVE('',#2039,#2032,#1353,.T.);
#2489=EDGE_CURVE('',#2041,#2041,#446,.T.);
#2490=EDGE_CURVE('',#2042,#2042,#447,.T.);
#2491=EDGE_CURVE('',#2042,#2041,#1354,.T.);
#2492=EDGE_CURVE('',#2043,#2043,#448,.T.);
#2493=EDGE_CURVE('',#2043,#2042,#1355,.T.);
#2494=EDGE_CURVE('',#2044,#2044,#449,.T.);
#2495=EDGE_CURVE('',#2044,#2043,#1356,.T.);
#2496=EDGE_CURVE('',#2045,#2045,#450,.T.);
#2497=EDGE_CURVE('',#2046,#2046,#451,.F.);
#2498=EDGE_CURVE('',#2046,#2045,#1357,.T.);
#2499=EDGE_CURVE('',#2047,#2047,#452,.F.);
#2500=EDGE_CURVE('',#2047,#2046,#1358,.T.);
#2501=EDGE_CURVE('',#2048,#2048,#453,.T.);
#2502=EDGE_CURVE('',#2048,#2047,#1359,.T.);
#2503=EDGE_CURVE('',#2049,#2050,#1360,.T.);
#2504=EDGE_CURVE('',#2050,#2051,#1361,.T.);
#2505=EDGE_CURVE('',#2051,#2052,#1362,.T.);
#2506=EDGE_CURVE('',#2049,#2052,#1363,.T.);
#2507=EDGE_CURVE('',#2050,#2053,#1364,.T.);
#2508=EDGE_CURVE('',#2053,#2054,#1365,.T.);
#2509=EDGE_CURVE('',#2054,#2051,#1366,.T.);
#2510=EDGE_CURVE('',#2053,#2055,#1367,.T.);
#2511=EDGE_CURVE('',#2055,#2056,#1368,.T.);
#2512=EDGE_CURVE('',#2056,#2054,#1369,.T.);
#2513=EDGE_CURVE('',#2055,#2057,#1370,.T.);
#2514=EDGE_CURVE('',#2057,#2058,#1371,.T.);
#2515=EDGE_CURVE('',#2058,#2056,#1372,.T.);
#2516=EDGE_CURVE('',#2057,#2059,#1373,.T.);
#2517=EDGE_CURVE('',#2059,#2060,#1374,.T.);
#2518=EDGE_CURVE('',#2060,#2058,#1375,.T.);
#2519=EDGE_CURVE('',#2059,#2049,#1376,.T.);
#2520=EDGE_CURVE('',#2052,#2060,#1377,.T.);
#2521=EDGE_CURVE('',#2061,#2061,#454,.T.);
#2522=EDGE_CURVE('',#2062,#2062,#455,.T.);
#2523=EDGE_CURVE('',#2062,#2061,#1378,.T.);
#2524=EDGE_CURVE('',#2063,#2063,#456,.T.);
#2525=EDGE_CURVE('',#2063,#2062,#1379,.T.);
#2526=EDGE_CURVE('',#2064,#2064,#457,.T.);
#2527=EDGE_CURVE('',#2064,#2063,#1380,.T.);
#2528=EDGE_CURVE('',#2065,#2065,#458,.T.);
#2529=EDGE_CURVE('',#2066,#2066,#459,.F.);
#2530=EDGE_CURVE('',#2066,#2065,#1381,.T.);
#2531=EDGE_CURVE('',#2067,#2067,#460,.F.);
#2532=EDGE_CURVE('',#2067,#2066,#1382,.T.);
#2533=EDGE_CURVE('',#2068,#2068,#461,.T.);
#2534=EDGE_CURVE('',#2068,#2067,#1383,.T.);
#2535=EDGE_CURVE('',#2069,#2070,#1384,.T.);
#2536=EDGE_CURVE('',#2070,#2071,#1385,.T.);
#2537=EDGE_CURVE('',#2071,#2072,#1386,.T.);
#2538=EDGE_CURVE('',#2069,#2072,#1387,.T.);
#2539=EDGE_CURVE('',#2070,#2073,#1388,.T.);
#2540=EDGE_CURVE('',#2073,#2074,#1389,.T.);
#2541=EDGE_CURVE('',#2074,#2071,#1390,.T.);
#2542=EDGE_CURVE('',#2073,#2075,#1391,.T.);
#2543=EDGE_CURVE('',#2075,#2076,#1392,.T.);
#2544=EDGE_CURVE('',#2076,#2074,#1393,.T.);
#2545=EDGE_CURVE('',#2075,#2077,#1394,.T.);
#2546=EDGE_CURVE('',#2077,#2078,#1395,.T.);
#2547=EDGE_CURVE('',#2078,#2076,#1396,.T.);
#2548=EDGE_CURVE('',#2077,#2079,#1397,.T.);
#2549=EDGE_CURVE('',#2079,#2080,#1398,.T.);
#2550=EDGE_CURVE('',#2080,#2078,#1399,.T.);
#2551=EDGE_CURVE('',#2079,#2069,#1400,.T.);
#2552=EDGE_CURVE('',#2072,#2080,#1401,.T.);
#2553=EDGE_CURVE('',#2081,#2081,#462,.T.);
#2554=EDGE_CURVE('',#2081,#2082,#1402,.T.);
#2555=EDGE_CURVE('',#2082,#2082,#463,.T.);
#2556=EDGE_CURVE('',#2083,#2083,#464,.T.);
#2557=EDGE_CURVE('',#2083,#2084,#1403,.T.);
#2558=EDGE_CURVE('',#2084,#2084,#465,.T.);
#2559=EDGE_CURVE('',#2085,#2086,#175,.T.);
#2560=EDGE_CURVE('',#2087,#2085,#176,.T.);
#2561=EDGE_CURVE('',#2087,#2088,#1404,.T.);
#2562=EDGE_CURVE('',#2088,#2088,#466,.T.);
#2563=EDGE_CURVE('',#2089,#2087,#177,.T.);
#2564=EDGE_CURVE('',#2090,#2089,#178,.T.);
#2565=EDGE_CURVE('',#2091,#2090,#179,.T.);
#2566=EDGE_CURVE('',#2086,#2091,#180,.T.);
#2567=EDGE_CURVE('',#2092,#2092,#467,.T.);
#2568=EDGE_CURVE('',#2092,#2093,#1405,.T.);
#2569=EDGE_CURVE('',#2094,#2093,#181,.T.);
#2570=EDGE_CURVE('',#2095,#2094,#182,.T.);
#2571=EDGE_CURVE('',#2096,#2095,#183,.T.);
#2572=EDGE_CURVE('',#2097,#2096,#184,.T.);
#2573=EDGE_CURVE('',#2098,#2097,#185,.T.);
#2574=EDGE_CURVE('',#2093,#2098,#186,.T.);
#2575=EDGE_CURVE('',#2089,#2098,#1406,.T.);
#2576=EDGE_CURVE('',#2090,#2097,#1407,.T.);
#2577=EDGE_CURVE('',#2087,#2093,#1408,.T.);
#2578=EDGE_CURVE('',#2085,#2094,#1409,.T.);
#2579=EDGE_CURVE('',#2099,#2099,#468,.F.);
#2580=EDGE_CURVE('',#2099,#2100,#1410,.T.);
#2581=EDGE_CURVE('',#2100,#2100,#469,.F.);
#2582=EDGE_CURVE('',#2086,#2095,#1411,.T.);
#2583=EDGE_CURVE('',#2091,#2096,#1412,.T.);
#2584=EDGE_CURVE('',#2101,#2101,#470,.T.);
#2585=EDGE_CURVE('',#2101,#2102,#1413,.T.);
#2586=EDGE_CURVE('',#2102,#2102,#471,.T.);
#2587=EDGE_CURVE('',#2103,#2103,#472,.T.);
#2588=EDGE_CURVE('',#2103,#2104,#1414,.T.);
#2589=EDGE_CURVE('',#2104,#2104,#473,.T.);
#2590=EDGE_CURVE('',#2105,#2105,#474,.T.);
#2591=EDGE_CURVE('',#2105,#2106,#1415,.T.);
#2592=EDGE_CURVE('',#2106,#2106,#475,.T.);
#2593=EDGE_CURVE('',#2107,#2107,#476,.T.);
#2594=EDGE_CURVE('',#2107,#2108,#1416,.T.);
#2595=EDGE_CURVE('',#2108,#2108,#477,.T.);
#2596=EDGE_CURVE('',#2109,#2110,#1417,.T.);
#2597=EDGE_CURVE('',#2110,#2111,#1418,.T.);
#2598=EDGE_CURVE('',#2112,#2111,#1419,.T.);
#2599=EDGE_CURVE('',#2109,#2112,#1420,.T.);
#2600=EDGE_CURVE('',#2113,#2109,#1421,.T.);
#2601=EDGE_CURVE('',#2114,#2112,#1422,.T.);
#2602=EDGE_CURVE('',#2113,#2114,#1423,.T.);
#2603=EDGE_CURVE('',#2115,#2113,#1424,.T.);
#2604=EDGE_CURVE('',#2116,#2114,#1425,.T.);
#2605=EDGE_CURVE('',#2115,#2116,#1426,.T.);
#2606=EDGE_CURVE('',#2110,#2115,#1427,.T.);
#2607=EDGE_CURVE('',#2111,#2116,#1428,.T.);
#2608=EDGE_CURVE('',#2117,#2117,#478,.T.);
#2609=EDGE_CURVE('',#2117,#2118,#1429,.T.);
#2610=EDGE_CURVE('',#2118,#2118,#479,.T.);
#2611=EDGE_CURVE('',#2119,#2119,#480,.T.);
#2612=EDGE_CURVE('',#2119,#2120,#1430,.T.);
#2613=EDGE_CURVE('',#2120,#2120,#481,.T.);
#2614=EDGE_CURVE('',#2121,#2122,#1431,.T.);
#2615=EDGE_CURVE('',#2123,#2121,#482,.T.);
#2616=EDGE_CURVE('',#2124,#2123,#1432,.T.);
#2617=EDGE_CURVE('',#2122,#2124,#483,.T.);
#2618=EDGE_CURVE('',#2121,#2125,#1433,.T.);
#2619=EDGE_CURVE('',#2126,#2125,#1434,.T.);
#2620=EDGE_CURVE('',#2123,#2126,#1435,.T.);
#2621=EDGE_CURVE('',#2122,#2127,#1436,.T.);
#2622=EDGE_CURVE('',#2125,#2127,#1437,.T.);
#2623=EDGE_CURVE('',#2128,#2126,#1438,.T.);
#2624=EDGE_CURVE('',#2124,#2128,#1439,.T.);
#2625=EDGE_CURVE('',#2127,#2128,#1440,.T.);
#2626=EDGE_CURVE('',#2129,#2129,#484,.F.);
#2627=EDGE_CURVE('',#2129,#2130,#1441,.T.);
#2628=EDGE_CURVE('',#2130,#2130,#485,.F.);
#2629=EDGE_CURVE('',#2131,#2131,#486,.F.);
#2630=EDGE_CURVE('',#2131,#2132,#1442,.T.);
#2631=EDGE_CURVE('',#2132,#2132,#487,.F.);
#2632=EDGE_CURVE('',#2133,#2134,#1443,.T.);
#2633=EDGE_CURVE('',#2134,#2135,#1444,.T.);
#2634=EDGE_CURVE('',#2135,#2136,#1445,.T.);
#2635=EDGE_CURVE('',#2133,#2136,#1446,.T.);
#2636=EDGE_CURVE('',#2134,#2137,#1447,.T.);
#2637=EDGE_CURVE('',#2137,#2138,#1448,.T.);
#2638=EDGE_CURVE('',#2138,#2135,#1449,.T.);
#2639=EDGE_CURVE('',#2137,#2139,#1450,.T.);
#2640=EDGE_CURVE('',#2139,#2140,#1451,.T.);
#2641=EDGE_CURVE('',#2140,#2138,#1452,.T.);
#2642=EDGE_CURVE('',#2139,#2141,#1453,.T.);
#2643=EDGE_CURVE('',#2141,#2142,#1454,.T.);
#2644=EDGE_CURVE('',#2142,#2140,#1455,.T.);
#2645=EDGE_CURVE('',#2141,#2143,#1456,.T.);
#2646=EDGE_CURVE('',#2143,#2144,#1457,.T.);
#2647=EDGE_CURVE('',#2144,#2142,#1458,.T.);
#2648=EDGE_CURVE('',#2143,#2133,#1459,.T.);
#2649=EDGE_CURVE('',#2136,#2144,#1460,.T.);
#2650=EDGE_CURVE('',#2145,#2145,#488,.T.);
#2651=EDGE_CURVE('',#2146,#2146,#489,.T.);
#2652=EDGE_CURVE('',#2147,#2147,#490,.T.);
#2653=EDGE_CURVE('',#2147,#2146,#1461,.T.);
#2654=EDGE_CURVE('',#2148,#2148,#491,.T.);
#2655=EDGE_CURVE('',#2148,#2147,#1462,.T.);
#2656=EDGE_CURVE('',#2149,#2149,#492,.T.);
#2657=EDGE_CURVE('',#2149,#2148,#1463,.T.);
#2658=EDGE_CURVE('',#2150,#2150,#493,.T.);
#2659=EDGE_CURVE('',#2151,#2151,#494,.F.);
#2660=EDGE_CURVE('',#2151,#2150,#1464,.T.);
#2661=EDGE_CURVE('',#2145,#2151,#1465,.T.);
#2662=EDGE_CURVE('',#2152,#2152,#495,.T.);
#2663=EDGE_CURVE('',#2152,#2153,#1466,.T.);
#2664=EDGE_CURVE('',#2153,#2153,#496,.T.);
#2665=EDGE_CURVE('',#2154,#2154,#497,.T.);
#2666=EDGE_CURVE('',#2154,#2155,#1467,.T.);
#2667=EDGE_CURVE('',#2155,#2155,#498,.T.);
#2668=EDGE_CURVE('',#2156,#2157,#187,.T.);
#2669=EDGE_CURVE('',#2158,#2156,#188,.T.);
#2670=EDGE_CURVE('',#2158,#2159,#1468,.T.);
#2671=EDGE_CURVE('',#2159,#2159,#499,.T.);
#2672=EDGE_CURVE('',#2160,#2158,#189,.T.);
#2673=EDGE_CURVE('',#2161,#2160,#190,.T.);
#2674=EDGE_CURVE('',#2162,#2161,#191,.T.);
#2675=EDGE_CURVE('',#2157,#2162,#192,.T.);
#2676=EDGE_CURVE('',#2163,#2163,#500,.T.);
#2677=EDGE_CURVE('',#2163,#2164,#1469,.T.);
#2678=EDGE_CURVE('',#2165,#2164,#193,.T.);
#2679=EDGE_CURVE('',#2166,#2165,#194,.T.);
#2680=EDGE_CURVE('',#2167,#2166,#195,.T.);
#2681=EDGE_CURVE('',#2168,#2167,#196,.T.);
#2682=EDGE_CURVE('',#2169,#2168,#197,.T.);
#2683=EDGE_CURVE('',#2164,#2169,#198,.T.);
#2684=EDGE_CURVE('',#2160,#2169,#1470,.T.);
#2685=EDGE_CURVE('',#2161,#2168,#1471,.T.);
#2686=EDGE_CURVE('',#2158,#2164,#1472,.T.);
#2687=EDGE_CURVE('',#2156,#2165,#1473,.T.);
#2688=EDGE_CURVE('',#2170,#2170,#501,.F.);
#2689=EDGE_CURVE('',#2170,#2171,#1474,.T.);
#2690=EDGE_CURVE('',#2171,#2171,#502,.F.);
#2691=EDGE_CURVE('',#2157,#2166,#1475,.T.);
#2692=EDGE_CURVE('',#2162,#2167,#1476,.T.);
#2693=EDGE_CURVE('',#2172,#2172,#503,.T.);
#2694=EDGE_CURVE('',#2172,#2173,#1477,.T.);
#2695=EDGE_CURVE('',#2173,#2173,#504,.T.);
#2696=ORIENTED_EDGE('',*,*,#2174,.F.);
#2697=ORIENTED_EDGE('',*,*,#2175,.F.);
#2698=ORIENTED_EDGE('',*,*,#2176,.F.);
#2699=ORIENTED_EDGE('',*,*,#2177,.T.);
#2700=ORIENTED_EDGE('',*,*,#2178,.F.);
#2701=ORIENTED_EDGE('',*,*,#2177,.F.);
#2702=ORIENTED_EDGE('',*,*,#2179,.F.);
#2703=ORIENTED_EDGE('',*,*,#2180,.T.);
#2704=ORIENTED_EDGE('',*,*,#2181,.F.);
#2705=ORIENTED_EDGE('',*,*,#2180,.F.);
#2706=ORIENTED_EDGE('',*,*,#2182,.F.);
#2707=ORIENTED_EDGE('',*,*,#2183,.T.);
#2708=ORIENTED_EDGE('',*,*,#2184,.F.);
#2709=ORIENTED_EDGE('',*,*,#2183,.F.);
#2710=ORIENTED_EDGE('',*,*,#2185,.F.);
#2711=ORIENTED_EDGE('',*,*,#2175,.T.);
#2712=ORIENTED_EDGE('',*,*,#2179,.T.);
#2713=ORIENTED_EDGE('',*,*,#2176,.T.);
#2714=ORIENTED_EDGE('',*,*,#2185,.T.);
#2715=ORIENTED_EDGE('',*,*,#2182,.T.);
#2716=ORIENTED_EDGE('',*,*,#2186,.F.);
#2717=ORIENTED_EDGE('',*,*,#2187,.F.);
#2718=ORIENTED_EDGE('',*,*,#2188,.F.);
#2719=ORIENTED_EDGE('',*,*,#2189,.T.);
#2720=ORIENTED_EDGE('',*,*,#2190,.F.);
#2721=ORIENTED_EDGE('',*,*,#2189,.F.);
#2722=ORIENTED_EDGE('',*,*,#2191,.F.);
#2723=ORIENTED_EDGE('',*,*,#2192,.T.);
#2724=ORIENTED_EDGE('',*,*,#2193,.F.);
#2725=ORIENTED_EDGE('',*,*,#2192,.F.);
#2726=ORIENTED_EDGE('',*,*,#2194,.F.);
#2727=ORIENTED_EDGE('',*,*,#2195,.T.);
#2728=ORIENTED_EDGE('',*,*,#2196,.F.);
#2729=ORIENTED_EDGE('',*,*,#2195,.F.);
#2730=ORIENTED_EDGE('',*,*,#2197,.F.);
#2731=ORIENTED_EDGE('',*,*,#2187,.T.);
#2732=ORIENTED_EDGE('',*,*,#2191,.T.);
#2733=ORIENTED_EDGE('',*,*,#2188,.T.);
#2734=ORIENTED_EDGE('',*,*,#2197,.T.);
#2735=ORIENTED_EDGE('',*,*,#2194,.T.);
#2736=ORIENTED_EDGE('',*,*,#2198,.F.);
#2737=ORIENTED_EDGE('',*,*,#2199,.T.);
#2738=ORIENTED_EDGE('',*,*,#2200,.F.);
#2739=ORIENTED_EDGE('',*,*,#2199,.F.);
#2740=ORIENTED_EDGE('',*,*,#2201,.F.);
#2741=ORIENTED_EDGE('',*,*,#2202,.T.);
#2742=ORIENTED_EDGE('',*,*,#2203,.F.);
#2743=ORIENTED_EDGE('',*,*,#2202,.F.);
#2744=ORIENTED_EDGE('',*,*,#2204,.F.);
#2745=ORIENTED_EDGE('',*,*,#2205,.T.);
#2746=ORIENTED_EDGE('',*,*,#2206,.F.);
#2747=ORIENTED_EDGE('',*,*,#2205,.F.);
#2748=ORIENTED_EDGE('',*,*,#2207,.F.);
#2749=ORIENTED_EDGE('',*,*,#2208,.T.);
#2750=ORIENTED_EDGE('',*,*,#2209,.F.);
#2751=ORIENTED_EDGE('',*,*,#2208,.F.);
#2752=ORIENTED_EDGE('',*,*,#2210,.F.);
#2753=ORIENTED_EDGE('',*,*,#2211,.T.);
#2754=ORIENTED_EDGE('',*,*,#2212,.F.);
#2755=ORIENTED_EDGE('',*,*,#2211,.F.);
#2756=ORIENTED_EDGE('',*,*,#2213,.F.);
#2757=ORIENTED_EDGE('',*,*,#2214,.T.);
#2758=ORIENTED_EDGE('',*,*,#2215,.F.);
#2759=ORIENTED_EDGE('',*,*,#2214,.F.);
#2760=ORIENTED_EDGE('',*,*,#2216,.F.);
#2761=ORIENTED_EDGE('',*,*,#2217,.T.);
#2762=ORIENTED_EDGE('',*,*,#2218,.F.);
#2763=ORIENTED_EDGE('',*,*,#2217,.F.);
#2764=ORIENTED_EDGE('',*,*,#2219,.F.);
#2765=ORIENTED_EDGE('',*,*,#2220,.T.);
#2766=ORIENTED_EDGE('',*,*,#2221,.F.);
#2767=ORIENTED_EDGE('',*,*,#2220,.F.);
#2768=ORIENTED_EDGE('',*,*,#2222,.F.);
#2769=ORIENTED_EDGE('',*,*,#2223,.T.);
#2770=ORIENTED_EDGE('',*,*,#2224,.F.);
#2771=ORIENTED_EDGE('',*,*,#2223,.F.);
#2772=ORIENTED_EDGE('',*,*,#2225,.F.);
#2773=ORIENTED_EDGE('',*,*,#2226,.T.);
#2774=ORIENTED_EDGE('',*,*,#2227,.F.);
#2775=ORIENTED_EDGE('',*,*,#2226,.F.);
#2776=ORIENTED_EDGE('',*,*,#2228,.F.);
#2777=ORIENTED_EDGE('',*,*,#2229,.T.);
#2778=ORIENTED_EDGE('',*,*,#2230,.F.);
#2779=ORIENTED_EDGE('',*,*,#2229,.F.);
#2780=ORIENTED_EDGE('',*,*,#2231,.F.);
#2781=ORIENTED_EDGE('',*,*,#2232,.T.);
#2782=ORIENTED_EDGE('',*,*,#2233,.F.);
#2783=ORIENTED_EDGE('',*,*,#2232,.F.);
#2784=ORIENTED_EDGE('',*,*,#2234,.T.);
#2785=ORIENTED_EDGE('',*,*,#2235,.T.);
#2786=ORIENTED_EDGE('',*,*,#2236,.F.);
#2787=ORIENTED_EDGE('',*,*,#2237,.F.);
#2788=ORIENTED_EDGE('',*,*,#2238,.T.);
#2789=ORIENTED_EDGE('',*,*,#2237,.T.);
#2790=ORIENTED_EDGE('',*,*,#2239,.F.);
#2791=ORIENTED_EDGE('',*,*,#2240,.F.);
#2792=ORIENTED_EDGE('',*,*,#2241,.T.);
#2793=ORIENTED_EDGE('',*,*,#2240,.T.);
#2794=ORIENTED_EDGE('',*,*,#2242,.F.);
#2795=ORIENTED_EDGE('',*,*,#2243,.F.);
#2796=ORIENTED_EDGE('',*,*,#2244,.T.);
#2797=ORIENTED_EDGE('',*,*,#2243,.T.);
#2798=ORIENTED_EDGE('',*,*,#2245,.F.);
#2799=ORIENTED_EDGE('',*,*,#2235,.F.);
#2800=ORIENTED_EDGE('',*,*,#2245,.T.);
#2801=ORIENTED_EDGE('',*,*,#2242,.T.);
#2802=ORIENTED_EDGE('',*,*,#2239,.T.);
#2803=ORIENTED_EDGE('',*,*,#2236,.T.);
#2804=ORIENTED_EDGE('',*,*,#2193,.T.);
#2805=ORIENTED_EDGE('',*,*,#2196,.T.);
#2806=ORIENTED_EDGE('',*,*,#2186,.T.);
#2807=ORIENTED_EDGE('',*,*,#2190,.T.);
#2808=ORIENTED_EDGE('',*,*,#2212,.T.);
#2809=ORIENTED_EDGE('',*,*,#2215,.T.);
#2810=ORIENTED_EDGE('',*,*,#2233,.T.);
#2811=ORIENTED_EDGE('',*,*,#2230,.T.);
#2812=ORIENTED_EDGE('',*,*,#2227,.T.);
#2813=ORIENTED_EDGE('',*,*,#2224,.T.);
#2814=ORIENTED_EDGE('',*,*,#2221,.T.);
#2815=ORIENTED_EDGE('',*,*,#2218,.T.);
#2816=ORIENTED_EDGE('',*,*,#2209,.T.);
#2817=ORIENTED_EDGE('',*,*,#2206,.T.);
#2818=ORIENTED_EDGE('',*,*,#2203,.T.);
#2819=ORIENTED_EDGE('',*,*,#2200,.T.);
#2820=ORIENTED_EDGE('',*,*,#2181,.T.);
#2821=ORIENTED_EDGE('',*,*,#2184,.T.);
#2822=ORIENTED_EDGE('',*,*,#2174,.T.);
#2823=ORIENTED_EDGE('',*,*,#2178,.T.);
#2824=ORIENTED_EDGE('',*,*,#2244,.F.);
#2825=ORIENTED_EDGE('',*,*,#2234,.F.);
#2826=ORIENTED_EDGE('',*,*,#2238,.F.);
#2827=ORIENTED_EDGE('',*,*,#2241,.F.);
#2828=ORIENTED_EDGE('',*,*,#2210,.T.);
#2829=ORIENTED_EDGE('',*,*,#2213,.T.);
#2830=ORIENTED_EDGE('',*,*,#2231,.T.);
#2831=ORIENTED_EDGE('',*,*,#2228,.T.);
#2832=ORIENTED_EDGE('',*,*,#2225,.T.);
#2833=ORIENTED_EDGE('',*,*,#2222,.T.);
#2834=ORIENTED_EDGE('',*,*,#2219,.T.);
#2835=ORIENTED_EDGE('',*,*,#2216,.T.);
#2836=ORIENTED_EDGE('',*,*,#2207,.T.);
#2837=ORIENTED_EDGE('',*,*,#2204,.T.);
#2838=ORIENTED_EDGE('',*,*,#2201,.T.);
#2839=ORIENTED_EDGE('',*,*,#2198,.T.);
#2840=ORIENTED_EDGE('',*,*,#2246,.F.);
#2841=ORIENTED_EDGE('',*,*,#2247,.T.);
#2842=ORIENTED_EDGE('',*,*,#2248,.F.);
#2843=ORIENTED_EDGE('',*,*,#2247,.F.);
#2844=ORIENTED_EDGE('',*,*,#2249,.F.);
#2845=ORIENTED_EDGE('',*,*,#2250,.T.);
#2846=ORIENTED_EDGE('',*,*,#2251,.F.);
#2847=ORIENTED_EDGE('',*,*,#2250,.F.);
#2848=ORIENTED_EDGE('',*,*,#2252,.T.);
#2849=ORIENTED_EDGE('',*,*,#2253,.T.);
#2850=ORIENTED_EDGE('',*,*,#2254,.F.);
#2851=ORIENTED_EDGE('',*,*,#2255,.F.);
#2852=ORIENTED_EDGE('',*,*,#2256,.T.);
#2853=ORIENTED_EDGE('',*,*,#2255,.T.);
#2854=ORIENTED_EDGE('',*,*,#2257,.F.);
#2855=ORIENTED_EDGE('',*,*,#2258,.F.);
#2856=ORIENTED_EDGE('',*,*,#2259,.T.);
#2857=ORIENTED_EDGE('',*,*,#2258,.T.);
#2858=ORIENTED_EDGE('',*,*,#2260,.F.);
#2859=ORIENTED_EDGE('',*,*,#2261,.F.);
#2860=ORIENTED_EDGE('',*,*,#2262,.T.);
#2861=ORIENTED_EDGE('',*,*,#2261,.T.);
#2862=ORIENTED_EDGE('',*,*,#2263,.F.);
#2863=ORIENTED_EDGE('',*,*,#2253,.F.);
#2864=ORIENTED_EDGE('',*,*,#2263,.T.);
#2865=ORIENTED_EDGE('',*,*,#2260,.T.);
#2866=ORIENTED_EDGE('',*,*,#2257,.T.);
#2867=ORIENTED_EDGE('',*,*,#2254,.T.);
#2868=ORIENTED_EDGE('',*,*,#2248,.T.);
#2869=ORIENTED_EDGE('',*,*,#2251,.T.);
#2870=ORIENTED_EDGE('',*,*,#2262,.F.);
#2871=ORIENTED_EDGE('',*,*,#2252,.F.);
#2872=ORIENTED_EDGE('',*,*,#2256,.F.);
#2873=ORIENTED_EDGE('',*,*,#2259,.F.);
#2874=ORIENTED_EDGE('',*,*,#2246,.T.);
#2875=ORIENTED_EDGE('',*,*,#2249,.T.);
#2876=ORIENTED_EDGE('',*,*,#2264,.T.);
#2877=ORIENTED_EDGE('',*,*,#2265,.T.);
#2878=ORIENTED_EDGE('',*,*,#2266,.F.);
#2879=ORIENTED_EDGE('',*,*,#2267,.F.);
#2880=ORIENTED_EDGE('',*,*,#2268,.T.);
#2881=ORIENTED_EDGE('',*,*,#2267,.T.);
#2882=ORIENTED_EDGE('',*,*,#2269,.F.);
#2883=ORIENTED_EDGE('',*,*,#2270,.F.);
#2884=ORIENTED_EDGE('',*,*,#2271,.T.);
#2885=ORIENTED_EDGE('',*,*,#2270,.T.);
#2886=ORIENTED_EDGE('',*,*,#2272,.F.);
#2887=ORIENTED_EDGE('',*,*,#2273,.F.);
#2888=ORIENTED_EDGE('',*,*,#2274,.T.);
#2889=ORIENTED_EDGE('',*,*,#2273,.T.);
#2890=ORIENTED_EDGE('',*,*,#2275,.F.);
#2891=ORIENTED_EDGE('',*,*,#2265,.F.);
#2892=ORIENTED_EDGE('',*,*,#2275,.T.);
#2893=ORIENTED_EDGE('',*,*,#2272,.T.);
#2894=ORIENTED_EDGE('',*,*,#2269,.T.);
#2895=ORIENTED_EDGE('',*,*,#2266,.T.);
#2896=ORIENTED_EDGE('',*,*,#2274,.F.);
#2897=ORIENTED_EDGE('',*,*,#2264,.F.);
#2898=ORIENTED_EDGE('',*,*,#2268,.F.);
#2899=ORIENTED_EDGE('',*,*,#2271,.F.);
#2900=ORIENTED_EDGE('',*,*,#2276,.F.);
#2901=ORIENTED_EDGE('',*,*,#2277,.T.);
#2902=ORIENTED_EDGE('',*,*,#2278,.F.);
#2903=ORIENTED_EDGE('',*,*,#2277,.F.);
#2904=ORIENTED_EDGE('',*,*,#2279,.F.);
#2905=ORIENTED_EDGE('',*,*,#2280,.T.);
#2906=ORIENTED_EDGE('',*,*,#2281,.F.);
#2907=ORIENTED_EDGE('',*,*,#2280,.F.);
#2908=ORIENTED_EDGE('',*,*,#2282,.T.);
#2909=ORIENTED_EDGE('',*,*,#2283,.T.);
#2910=ORIENTED_EDGE('',*,*,#2284,.F.);
#2911=ORIENTED_EDGE('',*,*,#2285,.F.);
#2912=ORIENTED_EDGE('',*,*,#2286,.T.);
#2913=ORIENTED_EDGE('',*,*,#2285,.T.);
#2914=ORIENTED_EDGE('',*,*,#2287,.F.);
#2915=ORIENTED_EDGE('',*,*,#2288,.F.);
#2916=ORIENTED_EDGE('',*,*,#2289,.T.);
#2917=ORIENTED_EDGE('',*,*,#2288,.T.);
#2918=ORIENTED_EDGE('',*,*,#2290,.F.);
#2919=ORIENTED_EDGE('',*,*,#2291,.F.);
#2920=ORIENTED_EDGE('',*,*,#2292,.T.);
#2921=ORIENTED_EDGE('',*,*,#2291,.T.);
#2922=ORIENTED_EDGE('',*,*,#2293,.F.);
#2923=ORIENTED_EDGE('',*,*,#2283,.F.);
#2924=ORIENTED_EDGE('',*,*,#2293,.T.);
#2925=ORIENTED_EDGE('',*,*,#2290,.T.);
#2926=ORIENTED_EDGE('',*,*,#2287,.T.);
#2927=ORIENTED_EDGE('',*,*,#2284,.T.);
#2928=ORIENTED_EDGE('',*,*,#2278,.T.);
#2929=ORIENTED_EDGE('',*,*,#2281,.T.);
#2930=ORIENTED_EDGE('',*,*,#2292,.F.);
#2931=ORIENTED_EDGE('',*,*,#2282,.F.);
#2932=ORIENTED_EDGE('',*,*,#2286,.F.);
#2933=ORIENTED_EDGE('',*,*,#2289,.F.);
#2934=ORIENTED_EDGE('',*,*,#2276,.T.);
#2935=ORIENTED_EDGE('',*,*,#2279,.T.);
#2936=ORIENTED_EDGE('',*,*,#2294,.T.);
#2937=ORIENTED_EDGE('',*,*,#2295,.T.);
#2938=ORIENTED_EDGE('',*,*,#2296,.F.);
#2939=ORIENTED_EDGE('',*,*,#2297,.F.);
#2940=ORIENTED_EDGE('',*,*,#2298,.T.);
#2941=ORIENTED_EDGE('',*,*,#2297,.T.);
#2942=ORIENTED_EDGE('',*,*,#2299,.F.);
#2943=ORIENTED_EDGE('',*,*,#2300,.F.);
#2944=ORIENTED_EDGE('',*,*,#2301,.T.);
#2945=ORIENTED_EDGE('',*,*,#2300,.T.);
#2946=ORIENTED_EDGE('',*,*,#2302,.F.);
#2947=ORIENTED_EDGE('',*,*,#2303,.F.);
#2948=ORIENTED_EDGE('',*,*,#2304,.T.);
#2949=ORIENTED_EDGE('',*,*,#2303,.T.);
#2950=ORIENTED_EDGE('',*,*,#2305,.F.);
#2951=ORIENTED_EDGE('',*,*,#2295,.F.);
#2952=ORIENTED_EDGE('',*,*,#2305,.T.);
#2953=ORIENTED_EDGE('',*,*,#2302,.T.);
#2954=ORIENTED_EDGE('',*,*,#2299,.T.);
#2955=ORIENTED_EDGE('',*,*,#2296,.T.);
#2956=ORIENTED_EDGE('',*,*,#2304,.F.);
#2957=ORIENTED_EDGE('',*,*,#2294,.F.);
#2958=ORIENTED_EDGE('',*,*,#2298,.F.);
#2959=ORIENTED_EDGE('',*,*,#2301,.F.);
#2960=ORIENTED_EDGE('',*,*,#2306,.F.);
#2961=ORIENTED_EDGE('',*,*,#2307,.F.);
#2962=ORIENTED_EDGE('',*,*,#2308,.T.);
#2963=ORIENTED_EDGE('',*,*,#2309,.F.);
#2964=ORIENTED_EDGE('',*,*,#2310,.F.);
#2965=ORIENTED_EDGE('',*,*,#2311,.F.);
#2966=ORIENTED_EDGE('',*,*,#2312,.T.);
#2967=ORIENTED_EDGE('',*,*,#2313,.F.);
#2968=ORIENTED_EDGE('',*,*,#2314,.F.);
#2969=ORIENTED_EDGE('',*,*,#2315,.F.);
#2970=ORIENTED_EDGE('',*,*,#2316,.T.);
#2971=ORIENTED_EDGE('',*,*,#2317,.T.);
#2972=ORIENTED_EDGE('',*,*,#2318,.F.);
#2973=ORIENTED_EDGE('',*,*,#2319,.F.);
#2974=ORIENTED_EDGE('',*,*,#2318,.T.);
#2975=ORIENTED_EDGE('',*,*,#2320,.T.);
#2976=ORIENTED_EDGE('',*,*,#2321,.F.);
#2977=ORIENTED_EDGE('',*,*,#2322,.F.);
#2978=ORIENTED_EDGE('',*,*,#2321,.T.);
#2979=ORIENTED_EDGE('',*,*,#2323,.T.);
#2980=ORIENTED_EDGE('',*,*,#2324,.F.);
#2981=ORIENTED_EDGE('',*,*,#2325,.F.);
#2982=ORIENTED_EDGE('',*,*,#2324,.T.);
#2983=ORIENTED_EDGE('',*,*,#2326,.T.);
#2984=ORIENTED_EDGE('',*,*,#2316,.F.);
#2985=ORIENTED_EDGE('',*,*,#2326,.F.);
#2986=ORIENTED_EDGE('',*,*,#2323,.F.);
#2987=ORIENTED_EDGE('',*,*,#2320,.F.);
#2988=ORIENTED_EDGE('',*,*,#2317,.F.);
#2989=ORIENTED_EDGE('',*,*,#2310,.T.);
#2990=ORIENTED_EDGE('',*,*,#2327,.F.);
#2991=ORIENTED_EDGE('',*,*,#2328,.F.);
#2992=ORIENTED_EDGE('',*,*,#2329,.F.);
#2993=ORIENTED_EDGE('',*,*,#2311,.T.);
#2994=ORIENTED_EDGE('',*,*,#2329,.T.);
#2995=ORIENTED_EDGE('',*,*,#2330,.F.);
#2996=ORIENTED_EDGE('',*,*,#2306,.T.);
#2997=ORIENTED_EDGE('',*,*,#2331,.F.);
#2998=ORIENTED_EDGE('',*,*,#2332,.F.);
#2999=ORIENTED_EDGE('',*,*,#2333,.F.);
#3000=ORIENTED_EDGE('',*,*,#2334,.F.);
#3001=ORIENTED_EDGE('',*,*,#2307,.T.);
#3002=ORIENTED_EDGE('',*,*,#2334,.T.);
#3003=ORIENTED_EDGE('',*,*,#2335,.F.);
#3004=ORIENTED_EDGE('',*,*,#2314,.T.);
#3005=ORIENTED_EDGE('',*,*,#2336,.F.);
#3006=ORIENTED_EDGE('',*,*,#2337,.F.);
#3007=ORIENTED_EDGE('',*,*,#2338,.F.);
#3008=ORIENTED_EDGE('',*,*,#2339,.F.);
#3009=ORIENTED_EDGE('',*,*,#2340,.F.);
#3010=ORIENTED_EDGE('',*,*,#2313,.T.);
#3011=ORIENTED_EDGE('',*,*,#2341,.T.);
#3012=ORIENTED_EDGE('',*,*,#2342,.T.);
#3013=ORIENTED_EDGE('',*,*,#2336,.T.);
#3014=ORIENTED_EDGE('',*,*,#2331,.T.);
#3015=ORIENTED_EDGE('',*,*,#2343,.F.);
#3016=ORIENTED_EDGE('',*,*,#2344,.F.);
#3017=ORIENTED_EDGE('',*,*,#2338,.T.);
#3018=ORIENTED_EDGE('',*,*,#2345,.F.);
#3019=ORIENTED_EDGE('',*,*,#2346,.F.);
#3020=ORIENTED_EDGE('',*,*,#2309,.T.);
#3021=ORIENTED_EDGE('',*,*,#2347,.T.);
#3022=ORIENTED_EDGE('',*,*,#2348,.T.);
#3023=ORIENTED_EDGE('',*,*,#2343,.T.);
#3024=ORIENTED_EDGE('',*,*,#2349,.F.);
#3025=ORIENTED_EDGE('',*,*,#2350,.T.);
#3026=ORIENTED_EDGE('',*,*,#2330,.T.);
#3027=ORIENTED_EDGE('',*,*,#2350,.F.);
#3028=ORIENTED_EDGE('',*,*,#2351,.F.);
#3029=ORIENTED_EDGE('',*,*,#2352,.T.);
#3030=ORIENTED_EDGE('',*,*,#2335,.T.);
#3031=ORIENTED_EDGE('',*,*,#2352,.F.);
#3032=ORIENTED_EDGE('',*,*,#2327,.T.);
#3033=ORIENTED_EDGE('',*,*,#2340,.T.);
#3034=ORIENTED_EDGE('',*,*,#2353,.T.);
#3035=ORIENTED_EDGE('',*,*,#2354,.T.);
#3036=ORIENTED_EDGE('',*,*,#2332,.T.);
#3037=ORIENTED_EDGE('',*,*,#2346,.T.);
#3038=ORIENTED_EDGE('',*,*,#2355,.T.);
#3039=ORIENTED_EDGE('',*,*,#2356,.T.);
#3040=ORIENTED_EDGE('',*,*,#2339,.T.);
#3041=ORIENTED_EDGE('',*,*,#2344,.T.);
#3042=ORIENTED_EDGE('',*,*,#2348,.F.);
#3043=ORIENTED_EDGE('',*,*,#2357,.F.);
#3044=ORIENTED_EDGE('',*,*,#2358,.T.);
#3045=ORIENTED_EDGE('',*,*,#2359,.T.);
#3046=ORIENTED_EDGE('',*,*,#2353,.F.);
#3047=ORIENTED_EDGE('',*,*,#2360,.T.);
#3048=ORIENTED_EDGE('',*,*,#2357,.T.);
#3049=ORIENTED_EDGE('',*,*,#2347,.F.);
#3050=ORIENTED_EDGE('',*,*,#2308,.F.);
#3051=ORIENTED_EDGE('',*,*,#2333,.T.);
#3052=ORIENTED_EDGE('',*,*,#2356,.F.);
#3053=ORIENTED_EDGE('',*,*,#2361,.F.);
#3054=ORIENTED_EDGE('',*,*,#2337,.T.);
#3055=ORIENTED_EDGE('',*,*,#2342,.F.);
#3056=ORIENTED_EDGE('',*,*,#2362,.F.);
#3057=ORIENTED_EDGE('',*,*,#2363,.T.);
#3058=ORIENTED_EDGE('',*,*,#2361,.T.);
#3059=ORIENTED_EDGE('',*,*,#2355,.F.);
#3060=ORIENTED_EDGE('',*,*,#2345,.T.);
#3061=ORIENTED_EDGE('',*,*,#2364,.T.);
#3062=ORIENTED_EDGE('',*,*,#2362,.T.);
#3063=ORIENTED_EDGE('',*,*,#2341,.F.);
#3064=ORIENTED_EDGE('',*,*,#2312,.F.);
#3065=ORIENTED_EDGE('',*,*,#2328,.T.);
#3066=ORIENTED_EDGE('',*,*,#2354,.F.);
#3067=ORIENTED_EDGE('',*,*,#2359,.F.);
#3068=ORIENTED_EDGE('',*,*,#2358,.F.);
#3069=ORIENTED_EDGE('',*,*,#2360,.F.);
#3070=ORIENTED_EDGE('',*,*,#2363,.F.);
#3071=ORIENTED_EDGE('',*,*,#2364,.F.);
#3072=ORIENTED_EDGE('',*,*,#2322,.T.);
#3073=ORIENTED_EDGE('',*,*,#2325,.T.);
#3074=ORIENTED_EDGE('',*,*,#2315,.T.);
#3075=ORIENTED_EDGE('',*,*,#2319,.T.);
#3076=ORIENTED_EDGE('',*,*,#2349,.T.);
#3077=ORIENTED_EDGE('',*,*,#2351,.T.);
#3078=ORIENTED_EDGE('',*,*,#2365,.F.);
#3079=ORIENTED_EDGE('',*,*,#2366,.F.);
#3080=ORIENTED_EDGE('',*,*,#2367,.T.);
#3081=ORIENTED_EDGE('',*,*,#2368,.F.);
#3082=ORIENTED_EDGE('',*,*,#2369,.F.);
#3083=ORIENTED_EDGE('',*,*,#2370,.F.);
#3084=ORIENTED_EDGE('',*,*,#2371,.T.);
#3085=ORIENTED_EDGE('',*,*,#2372,.F.);
#3086=ORIENTED_EDGE('',*,*,#2373,.F.);
#3087=ORIENTED_EDGE('',*,*,#2374,.F.);
#3088=ORIENTED_EDGE('',*,*,#2375,.T.);
#3089=ORIENTED_EDGE('',*,*,#2376,.T.);
#3090=ORIENTED_EDGE('',*,*,#2377,.F.);
#3091=ORIENTED_EDGE('',*,*,#2378,.F.);
#3092=ORIENTED_EDGE('',*,*,#2377,.T.);
#3093=ORIENTED_EDGE('',*,*,#2379,.T.);
#3094=ORIENTED_EDGE('',*,*,#2380,.F.);
#3095=ORIENTED_EDGE('',*,*,#2381,.F.);
#3096=ORIENTED_EDGE('',*,*,#2380,.T.);
#3097=ORIENTED_EDGE('',*,*,#2382,.T.);
#3098=ORIENTED_EDGE('',*,*,#2383,.F.);
#3099=ORIENTED_EDGE('',*,*,#2384,.F.);
#3100=ORIENTED_EDGE('',*,*,#2383,.T.);
#3101=ORIENTED_EDGE('',*,*,#2385,.T.);
#3102=ORIENTED_EDGE('',*,*,#2375,.F.);
#3103=ORIENTED_EDGE('',*,*,#2385,.F.);
#3104=ORIENTED_EDGE('',*,*,#2382,.F.);
#3105=ORIENTED_EDGE('',*,*,#2379,.F.);
#3106=ORIENTED_EDGE('',*,*,#2376,.F.);
#3107=ORIENTED_EDGE('',*,*,#2369,.T.);
#3108=ORIENTED_EDGE('',*,*,#2386,.F.);
#3109=ORIENTED_EDGE('',*,*,#2387,.F.);
#3110=ORIENTED_EDGE('',*,*,#2388,.F.);
#3111=ORIENTED_EDGE('',*,*,#2370,.T.);
#3112=ORIENTED_EDGE('',*,*,#2388,.T.);
#3113=ORIENTED_EDGE('',*,*,#2389,.F.);
#3114=ORIENTED_EDGE('',*,*,#2365,.T.);
#3115=ORIENTED_EDGE('',*,*,#2390,.F.);
#3116=ORIENTED_EDGE('',*,*,#2391,.F.);
#3117=ORIENTED_EDGE('',*,*,#2392,.F.);
#3118=ORIENTED_EDGE('',*,*,#2393,.F.);
#3119=ORIENTED_EDGE('',*,*,#2366,.T.);
#3120=ORIENTED_EDGE('',*,*,#2393,.T.);
#3121=ORIENTED_EDGE('',*,*,#2394,.F.);
#3122=ORIENTED_EDGE('',*,*,#2373,.T.);
#3123=ORIENTED_EDGE('',*,*,#2395,.F.);
#3124=ORIENTED_EDGE('',*,*,#2396,.F.);
#3125=ORIENTED_EDGE('',*,*,#2397,.F.);
#3126=ORIENTED_EDGE('',*,*,#2398,.F.);
#3127=ORIENTED_EDGE('',*,*,#2399,.F.);
#3128=ORIENTED_EDGE('',*,*,#2372,.T.);
#3129=ORIENTED_EDGE('',*,*,#2400,.T.);
#3130=ORIENTED_EDGE('',*,*,#2401,.T.);
#3131=ORIENTED_EDGE('',*,*,#2395,.T.);
#3132=ORIENTED_EDGE('',*,*,#2390,.T.);
#3133=ORIENTED_EDGE('',*,*,#2402,.F.);
#3134=ORIENTED_EDGE('',*,*,#2403,.F.);
#3135=ORIENTED_EDGE('',*,*,#2397,.T.);
#3136=ORIENTED_EDGE('',*,*,#2404,.F.);
#3137=ORIENTED_EDGE('',*,*,#2405,.F.);
#3138=ORIENTED_EDGE('',*,*,#2368,.T.);
#3139=ORIENTED_EDGE('',*,*,#2406,.T.);
#3140=ORIENTED_EDGE('',*,*,#2407,.T.);
#3141=ORIENTED_EDGE('',*,*,#2402,.T.);
#3142=ORIENTED_EDGE('',*,*,#2408,.F.);
#3143=ORIENTED_EDGE('',*,*,#2409,.T.);
#3144=ORIENTED_EDGE('',*,*,#2389,.T.);
#3145=ORIENTED_EDGE('',*,*,#2409,.F.);
#3146=ORIENTED_EDGE('',*,*,#2410,.F.);
#3147=ORIENTED_EDGE('',*,*,#2411,.T.);
#3148=ORIENTED_EDGE('',*,*,#2394,.T.);
#3149=ORIENTED_EDGE('',*,*,#2411,.F.);
#3150=ORIENTED_EDGE('',*,*,#2386,.T.);
#3151=ORIENTED_EDGE('',*,*,#2399,.T.);
#3152=ORIENTED_EDGE('',*,*,#2412,.T.);
#3153=ORIENTED_EDGE('',*,*,#2413,.T.);
#3154=ORIENTED_EDGE('',*,*,#2391,.T.);
#3155=ORIENTED_EDGE('',*,*,#2405,.T.);
#3156=ORIENTED_EDGE('',*,*,#2414,.T.);
#3157=ORIENTED_EDGE('',*,*,#2415,.T.);
#3158=ORIENTED_EDGE('',*,*,#2398,.T.);
#3159=ORIENTED_EDGE('',*,*,#2403,.T.);
#3160=ORIENTED_EDGE('',*,*,#2407,.F.);
#3161=ORIENTED_EDGE('',*,*,#2416,.F.);
#3162=ORIENTED_EDGE('',*,*,#2417,.T.);
#3163=ORIENTED_EDGE('',*,*,#2418,.T.);
#3164=ORIENTED_EDGE('',*,*,#2412,.F.);
#3165=ORIENTED_EDGE('',*,*,#2419,.T.);
#3166=ORIENTED_EDGE('',*,*,#2416,.T.);
#3167=ORIENTED_EDGE('',*,*,#2406,.F.);
#3168=ORIENTED_EDGE('',*,*,#2367,.F.);
#3169=ORIENTED_EDGE('',*,*,#2392,.T.);
#3170=ORIENTED_EDGE('',*,*,#2415,.F.);
#3171=ORIENTED_EDGE('',*,*,#2420,.F.);
#3172=ORIENTED_EDGE('',*,*,#2396,.T.);
#3173=ORIENTED_EDGE('',*,*,#2401,.F.);
#3174=ORIENTED_EDGE('',*,*,#2421,.F.);
#3175=ORIENTED_EDGE('',*,*,#2422,.T.);
#3176=ORIENTED_EDGE('',*,*,#2420,.T.);
#3177=ORIENTED_EDGE('',*,*,#2414,.F.);
#3178=ORIENTED_EDGE('',*,*,#2404,.T.);
#3179=ORIENTED_EDGE('',*,*,#2423,.T.);
#3180=ORIENTED_EDGE('',*,*,#2421,.T.);
#3181=ORIENTED_EDGE('',*,*,#2400,.F.);
#3182=ORIENTED_EDGE('',*,*,#2371,.F.);
#3183=ORIENTED_EDGE('',*,*,#2387,.T.);
#3184=ORIENTED_EDGE('',*,*,#2413,.F.);
#3185=ORIENTED_EDGE('',*,*,#2418,.F.);
#3186=ORIENTED_EDGE('',*,*,#2417,.F.);
#3187=ORIENTED_EDGE('',*,*,#2419,.F.);
#3188=ORIENTED_EDGE('',*,*,#2422,.F.);
#3189=ORIENTED_EDGE('',*,*,#2423,.F.);
#3190=ORIENTED_EDGE('',*,*,#2381,.T.);
#3191=ORIENTED_EDGE('',*,*,#2384,.T.);
#3192=ORIENTED_EDGE('',*,*,#2374,.T.);
#3193=ORIENTED_EDGE('',*,*,#2378,.T.);
#3194=ORIENTED_EDGE('',*,*,#2408,.T.);
#3195=ORIENTED_EDGE('',*,*,#2410,.T.);
#3196=ORIENTED_EDGE('',*,*,#2424,.F.);
#3197=ORIENTED_EDGE('',*,*,#2425,.T.);
#3198=ORIENTED_EDGE('',*,*,#2426,.F.);
#3199=ORIENTED_EDGE('',*,*,#2425,.F.);
#3200=ORIENTED_EDGE('',*,*,#2427,.T.);
#3201=ORIENTED_EDGE('',*,*,#2428,.F.);
#3202=ORIENTED_EDGE('',*,*,#2429,.F.);
#3203=ORIENTED_EDGE('',*,*,#2430,.F.);
#3204=ORIENTED_EDGE('',*,*,#2431,.F.);
#3205=ORIENTED_EDGE('',*,*,#2432,.F.);
#3206=ORIENTED_EDGE('',*,*,#2433,.T.);
#3207=ORIENTED_EDGE('',*,*,#2434,.F.);
#3208=ORIENTED_EDGE('',*,*,#2432,.T.);
#3209=ORIENTED_EDGE('',*,*,#2430,.T.);
#3210=ORIENTED_EDGE('',*,*,#2435,.F.);
#3211=ORIENTED_EDGE('',*,*,#2436,.T.);
#3212=ORIENTED_EDGE('',*,*,#2437,.F.);
#3213=ORIENTED_EDGE('',*,*,#2438,.F.);
#3214=ORIENTED_EDGE('',*,*,#2439,.F.);
#3215=ORIENTED_EDGE('',*,*,#2440,.F.);
#3216=ORIENTED_EDGE('',*,*,#2441,.F.);
#3217=ORIENTED_EDGE('',*,*,#2442,.T.);
#3218=ORIENTED_EDGE('',*,*,#2443,.F.);
#3219=ORIENTED_EDGE('',*,*,#2441,.T.);
#3220=ORIENTED_EDGE('',*,*,#2439,.T.);
#3221=ORIENTED_EDGE('',*,*,#2444,.F.);
#3222=ORIENTED_EDGE('',*,*,#2437,.T.);
#3223=ORIENTED_EDGE('',*,*,#2445,.T.);
#3224=ORIENTED_EDGE('',*,*,#2446,.T.);
#3225=ORIENTED_EDGE('',*,*,#2447,.T.);
#3226=ORIENTED_EDGE('',*,*,#2428,.T.);
#3227=ORIENTED_EDGE('',*,*,#2448,.T.);
#3228=ORIENTED_EDGE('',*,*,#2443,.T.);
#3229=ORIENTED_EDGE('',*,*,#2449,.T.);
#3230=ORIENTED_EDGE('',*,*,#2434,.T.);
#3231=ORIENTED_EDGE('',*,*,#2450,.T.);
#3232=ORIENTED_EDGE('',*,*,#2451,.T.);
#3233=ORIENTED_EDGE('',*,*,#2452,.T.);
#3234=ORIENTED_EDGE('',*,*,#2453,.F.);
#3235=ORIENTED_EDGE('',*,*,#2454,.T.);
#3236=ORIENTED_EDGE('',*,*,#2435,.T.);
#3237=ORIENTED_EDGE('',*,*,#2454,.F.);
#3238=ORIENTED_EDGE('',*,*,#2455,.F.);
#3239=ORIENTED_EDGE('',*,*,#2456,.T.);
#3240=ORIENTED_EDGE('',*,*,#2444,.T.);
#3241=ORIENTED_EDGE('',*,*,#2456,.F.);
#3242=ORIENTED_EDGE('',*,*,#2457,.T.);
#3243=ORIENTED_EDGE('',*,*,#2458,.T.);
#3244=ORIENTED_EDGE('',*,*,#2446,.F.);
#3245=ORIENTED_EDGE('',*,*,#2459,.F.);
#3246=ORIENTED_EDGE('',*,*,#2460,.T.);
#3247=ORIENTED_EDGE('',*,*,#2459,.T.);
#3248=ORIENTED_EDGE('',*,*,#2445,.F.);
#3249=ORIENTED_EDGE('',*,*,#2436,.F.);
#3250=ORIENTED_EDGE('',*,*,#2440,.T.);
#3251=ORIENTED_EDGE('',*,*,#2448,.F.);
#3252=ORIENTED_EDGE('',*,*,#2427,.F.);
#3253=ORIENTED_EDGE('',*,*,#2431,.T.);
#3254=ORIENTED_EDGE('',*,*,#2452,.F.);
#3255=ORIENTED_EDGE('',*,*,#2461,.F.);
#3256=ORIENTED_EDGE('',*,*,#2426,.T.);
#3257=ORIENTED_EDGE('',*,*,#2462,.T.);
#3258=ORIENTED_EDGE('',*,*,#2461,.T.);
#3259=ORIENTED_EDGE('',*,*,#2451,.F.);
#3260=ORIENTED_EDGE('',*,*,#2463,.F.);
#3261=ORIENTED_EDGE('',*,*,#2464,.T.);
#3262=ORIENTED_EDGE('',*,*,#2463,.T.);
#3263=ORIENTED_EDGE('',*,*,#2450,.F.);
#3264=ORIENTED_EDGE('',*,*,#2433,.F.);
#3265=ORIENTED_EDGE('',*,*,#2429,.T.);
#3266=ORIENTED_EDGE('',*,*,#2449,.F.);
#3267=ORIENTED_EDGE('',*,*,#2442,.F.);
#3268=ORIENTED_EDGE('',*,*,#2438,.T.);
#3269=ORIENTED_EDGE('',*,*,#2447,.F.);
#3270=ORIENTED_EDGE('',*,*,#2458,.F.);
#3271=ORIENTED_EDGE('',*,*,#2424,.T.);
#3272=ORIENTED_EDGE('',*,*,#2464,.F.);
#3273=ORIENTED_EDGE('',*,*,#2457,.F.);
#3274=ORIENTED_EDGE('',*,*,#2460,.F.);
#3275=ORIENTED_EDGE('',*,*,#2462,.F.);
#3276=ORIENTED_EDGE('',*,*,#2453,.T.);
#3277=ORIENTED_EDGE('',*,*,#2455,.T.);
#3278=ORIENTED_EDGE('',*,*,#2465,.F.);
#3279=ORIENTED_EDGE('',*,*,#2466,.F.);
#3280=ORIENTED_EDGE('',*,*,#2467,.F.);
#3281=ORIENTED_EDGE('',*,*,#2468,.F.);
#3282=ORIENTED_EDGE('',*,*,#2469,.F.);
#3283=ORIENTED_EDGE('',*,*,#2470,.F.);
#3284=ORIENTED_EDGE('',*,*,#2471,.F.);
#3285=ORIENTED_EDGE('',*,*,#2472,.F.);
#3286=ORIENTED_EDGE('',*,*,#2469,.T.);
#3287=ORIENTED_EDGE('',*,*,#2473,.T.);
#3288=ORIENTED_EDGE('',*,*,#2474,.T.);
#3289=ORIENTED_EDGE('',*,*,#2475,.T.);
#3290=ORIENTED_EDGE('',*,*,#2468,.T.);
#3291=ORIENTED_EDGE('',*,*,#2476,.F.);
#3292=ORIENTED_EDGE('',*,*,#2477,.T.);
#3293=ORIENTED_EDGE('',*,*,#2473,.F.);
#3294=ORIENTED_EDGE('',*,*,#2467,.T.);
#3295=ORIENTED_EDGE('',*,*,#2478,.T.);
#3296=ORIENTED_EDGE('',*,*,#2479,.T.);
#3297=ORIENTED_EDGE('',*,*,#2476,.T.);
#3298=ORIENTED_EDGE('',*,*,#2466,.T.);
#3299=ORIENTED_EDGE('',*,*,#2480,.F.);
#3300=ORIENTED_EDGE('',*,*,#2481,.T.);
#3301=ORIENTED_EDGE('',*,*,#2478,.F.);
#3302=ORIENTED_EDGE('',*,*,#2482,.F.);
#3303=ORIENTED_EDGE('',*,*,#2483,.F.);
#3304=ORIENTED_EDGE('',*,*,#2474,.F.);
#3305=ORIENTED_EDGE('',*,*,#2477,.F.);
#3306=ORIENTED_EDGE('',*,*,#2479,.F.);
#3307=ORIENTED_EDGE('',*,*,#2481,.F.);
#3308=ORIENTED_EDGE('',*,*,#2484,.F.);
#3309=ORIENTED_EDGE('',*,*,#2485,.F.);
#3310=ORIENTED_EDGE('',*,*,#2470,.T.);
#3311=ORIENTED_EDGE('',*,*,#2475,.F.);
#3312=ORIENTED_EDGE('',*,*,#2483,.T.);
#3313=ORIENTED_EDGE('',*,*,#2486,.F.);
#3314=ORIENTED_EDGE('',*,*,#2465,.T.);
#3315=ORIENTED_EDGE('',*,*,#2487,.T.);
#3316=ORIENTED_EDGE('',*,*,#2484,.T.);
#3317=ORIENTED_EDGE('',*,*,#2480,.T.);
#3318=ORIENTED_EDGE('',*,*,#2471,.T.);
#3319=ORIENTED_EDGE('',*,*,#2486,.T.);
#3320=ORIENTED_EDGE('',*,*,#2482,.T.);
#3321=ORIENTED_EDGE('',*,*,#2488,.T.);
#3322=ORIENTED_EDGE('',*,*,#2472,.T.);
#3323=ORIENTED_EDGE('',*,*,#2488,.F.);
#3324=ORIENTED_EDGE('',*,*,#2485,.T.);
#3325=ORIENTED_EDGE('',*,*,#2487,.F.);
#3326=ORIENTED_EDGE('',*,*,#2489,.F.);
#3327=ORIENTED_EDGE('',*,*,#2490,.F.);
#3328=ORIENTED_EDGE('',*,*,#2491,.T.);
#3329=ORIENTED_EDGE('',*,*,#2489,.T.);
#3330=ORIENTED_EDGE('',*,*,#2491,.F.);
#3331=ORIENTED_EDGE('',*,*,#2492,.F.);
#3332=ORIENTED_EDGE('',*,*,#2493,.T.);
#3333=ORIENTED_EDGE('',*,*,#2490,.T.);
#3334=ORIENTED_EDGE('',*,*,#2493,.F.);
#3335=ORIENTED_EDGE('',*,*,#2494,.F.);
#3336=ORIENTED_EDGE('',*,*,#2495,.T.);
#3337=ORIENTED_EDGE('',*,*,#2492,.T.);
#3338=ORIENTED_EDGE('',*,*,#2495,.F.);
#3339=ORIENTED_EDGE('',*,*,#2494,.T.);
#3340=ORIENTED_EDGE('',*,*,#2496,.F.);
#3341=ORIENTED_EDGE('',*,*,#2497,.F.);
#3342=ORIENTED_EDGE('',*,*,#2498,.T.);
#3343=ORIENTED_EDGE('',*,*,#2496,.T.);
#3344=ORIENTED_EDGE('',*,*,#2498,.F.);
#3345=ORIENTED_EDGE('',*,*,#2499,.F.);
#3346=ORIENTED_EDGE('',*,*,#2500,.T.);
#3347=ORIENTED_EDGE('',*,*,#2497,.T.);
#3348=ORIENTED_EDGE('',*,*,#2500,.F.);
#3349=ORIENTED_EDGE('',*,*,#2501,.F.);
#3350=ORIENTED_EDGE('',*,*,#2502,.T.);
#3351=ORIENTED_EDGE('',*,*,#2499,.T.);
#3352=ORIENTED_EDGE('',*,*,#2502,.F.);
#3353=ORIENTED_EDGE('',*,*,#2501,.T.);
#3354=ORIENTED_EDGE('',*,*,#2503,.T.);
#3355=ORIENTED_EDGE('',*,*,#2504,.T.);
#3356=ORIENTED_EDGE('',*,*,#2505,.T.);
#3357=ORIENTED_EDGE('',*,*,#2506,.F.);
#3358=ORIENTED_EDGE('',*,*,#2507,.T.);
#3359=ORIENTED_EDGE('',*,*,#2508,.T.);
#3360=ORIENTED_EDGE('',*,*,#2509,.T.);
#3361=ORIENTED_EDGE('',*,*,#2504,.F.);
#3362=ORIENTED_EDGE('',*,*,#2510,.T.);
#3363=ORIENTED_EDGE('',*,*,#2511,.T.);
#3364=ORIENTED_EDGE('',*,*,#2512,.T.);
#3365=ORIENTED_EDGE('',*,*,#2508,.F.);
#3366=ORIENTED_EDGE('',*,*,#2513,.T.);
#3367=ORIENTED_EDGE('',*,*,#2514,.T.);
#3368=ORIENTED_EDGE('',*,*,#2515,.T.);
#3369=ORIENTED_EDGE('',*,*,#2511,.F.);
#3370=ORIENTED_EDGE('',*,*,#2516,.T.);
#3371=ORIENTED_EDGE('',*,*,#2517,.T.);
#3372=ORIENTED_EDGE('',*,*,#2518,.T.);
#3373=ORIENTED_EDGE('',*,*,#2514,.F.);
#3374=ORIENTED_EDGE('',*,*,#2519,.T.);
#3375=ORIENTED_EDGE('',*,*,#2506,.T.);
#3376=ORIENTED_EDGE('',*,*,#2520,.T.);
#3377=ORIENTED_EDGE('',*,*,#2517,.F.);
#3378=ORIENTED_EDGE('',*,*,#2519,.F.);
#3379=ORIENTED_EDGE('',*,*,#2516,.F.);
#3380=ORIENTED_EDGE('',*,*,#2513,.F.);
#3381=ORIENTED_EDGE('',*,*,#2510,.F.);
#3382=ORIENTED_EDGE('',*,*,#2507,.F.);
#3383=ORIENTED_EDGE('',*,*,#2503,.F.);
#3384=ORIENTED_EDGE('',*,*,#2520,.F.);
#3385=ORIENTED_EDGE('',*,*,#2505,.F.);
#3386=ORIENTED_EDGE('',*,*,#2509,.F.);
#3387=ORIENTED_EDGE('',*,*,#2512,.F.);
#3388=ORIENTED_EDGE('',*,*,#2515,.F.);
#3389=ORIENTED_EDGE('',*,*,#2518,.F.);
#3390=ORIENTED_EDGE('',*,*,#2521,.F.);
#3391=ORIENTED_EDGE('',*,*,#2522,.F.);
#3392=ORIENTED_EDGE('',*,*,#2523,.T.);
#3393=ORIENTED_EDGE('',*,*,#2521,.T.);
#3394=ORIENTED_EDGE('',*,*,#2523,.F.);
#3395=ORIENTED_EDGE('',*,*,#2524,.F.);
#3396=ORIENTED_EDGE('',*,*,#2525,.T.);
#3397=ORIENTED_EDGE('',*,*,#2522,.T.);
#3398=ORIENTED_EDGE('',*,*,#2525,.F.);
#3399=ORIENTED_EDGE('',*,*,#2526,.F.);
#3400=ORIENTED_EDGE('',*,*,#2527,.T.);
#3401=ORIENTED_EDGE('',*,*,#2524,.T.);
#3402=ORIENTED_EDGE('',*,*,#2527,.F.);
#3403=ORIENTED_EDGE('',*,*,#2526,.T.);
#3404=ORIENTED_EDGE('',*,*,#2528,.F.);
#3405=ORIENTED_EDGE('',*,*,#2529,.F.);
#3406=ORIENTED_EDGE('',*,*,#2530,.T.);
#3407=ORIENTED_EDGE('',*,*,#2528,.T.);
#3408=ORIENTED_EDGE('',*,*,#2530,.F.);
#3409=ORIENTED_EDGE('',*,*,#2531,.F.);
#3410=ORIENTED_EDGE('',*,*,#2532,.T.);
#3411=ORIENTED_EDGE('',*,*,#2529,.T.);
#3412=ORIENTED_EDGE('',*,*,#2532,.F.);
#3413=ORIENTED_EDGE('',*,*,#2533,.F.);
#3414=ORIENTED_EDGE('',*,*,#2534,.T.);
#3415=ORIENTED_EDGE('',*,*,#2531,.T.);
#3416=ORIENTED_EDGE('',*,*,#2534,.F.);
#3417=ORIENTED_EDGE('',*,*,#2533,.T.);
#3418=ORIENTED_EDGE('',*,*,#2535,.T.);
#3419=ORIENTED_EDGE('',*,*,#2536,.T.);
#3420=ORIENTED_EDGE('',*,*,#2537,.T.);
#3421=ORIENTED_EDGE('',*,*,#2538,.F.);
#3422=ORIENTED_EDGE('',*,*,#2539,.T.);
#3423=ORIENTED_EDGE('',*,*,#2540,.T.);
#3424=ORIENTED_EDGE('',*,*,#2541,.T.);
#3425=ORIENTED_EDGE('',*,*,#2536,.F.);
#3426=ORIENTED_EDGE('',*,*,#2542,.T.);
#3427=ORIENTED_EDGE('',*,*,#2543,.T.);
#3428=ORIENTED_EDGE('',*,*,#2544,.T.);
#3429=ORIENTED_EDGE('',*,*,#2540,.F.);
#3430=ORIENTED_EDGE('',*,*,#2545,.T.);
#3431=ORIENTED_EDGE('',*,*,#2546,.T.);
#3432=ORIENTED_EDGE('',*,*,#2547,.T.);
#3433=ORIENTED_EDGE('',*,*,#2543,.F.);
#3434=ORIENTED_EDGE('',*,*,#2548,.T.);
#3435=ORIENTED_EDGE('',*,*,#2549,.T.);
#3436=ORIENTED_EDGE('',*,*,#2550,.T.);
#3437=ORIENTED_EDGE('',*,*,#2546,.F.);
#3438=ORIENTED_EDGE('',*,*,#2551,.T.);
#3439=ORIENTED_EDGE('',*,*,#2538,.T.);
#3440=ORIENTED_EDGE('',*,*,#2552,.T.);
#3441=ORIENTED_EDGE('',*,*,#2549,.F.);
#3442=ORIENTED_EDGE('',*,*,#2551,.F.);
#3443=ORIENTED_EDGE('',*,*,#2548,.F.);
#3444=ORIENTED_EDGE('',*,*,#2545,.F.);
#3445=ORIENTED_EDGE('',*,*,#2542,.F.);
#3446=ORIENTED_EDGE('',*,*,#2539,.F.);
#3447=ORIENTED_EDGE('',*,*,#2535,.F.);
#3448=ORIENTED_EDGE('',*,*,#2552,.F.);
#3449=ORIENTED_EDGE('',*,*,#2537,.F.);
#3450=ORIENTED_EDGE('',*,*,#2541,.F.);
#3451=ORIENTED_EDGE('',*,*,#2544,.F.);
#3452=ORIENTED_EDGE('',*,*,#2547,.F.);
#3453=ORIENTED_EDGE('',*,*,#2550,.F.);
#3454=ORIENTED_EDGE('',*,*,#2553,.F.);
#3455=ORIENTED_EDGE('',*,*,#2554,.T.);
#3456=ORIENTED_EDGE('',*,*,#2555,.T.);
#3457=ORIENTED_EDGE('',*,*,#2554,.F.);
#3458=ORIENTED_EDGE('',*,*,#2556,.F.);
#3459=ORIENTED_EDGE('',*,*,#2557,.T.);
#3460=ORIENTED_EDGE('',*,*,#2558,.T.);
#3461=ORIENTED_EDGE('',*,*,#2557,.F.);
#3462=ORIENTED_EDGE('',*,*,#2556,.T.);
#3463=ORIENTED_EDGE('',*,*,#2553,.T.);
#3464=ORIENTED_EDGE('',*,*,#2558,.F.);
#3465=ORIENTED_EDGE('',*,*,#2555,.F.);
#3466=ORIENTED_EDGE('',*,*,#2559,.F.);
#3467=ORIENTED_EDGE('',*,*,#2560,.F.);
#3468=ORIENTED_EDGE('',*,*,#2561,.T.);
#3469=ORIENTED_EDGE('',*,*,#2562,.F.);
#3470=ORIENTED_EDGE('',*,*,#2561,.F.);
#3471=ORIENTED_EDGE('',*,*,#2563,.F.);
#3472=ORIENTED_EDGE('',*,*,#2564,.F.);
#3473=ORIENTED_EDGE('',*,*,#2565,.F.);
#3474=ORIENTED_EDGE('',*,*,#2566,.F.);
#3475=ORIENTED_EDGE('',*,*,#2567,.F.);
#3476=ORIENTED_EDGE('',*,*,#2568,.T.);
#3477=ORIENTED_EDGE('',*,*,#2569,.F.);
#3478=ORIENTED_EDGE('',*,*,#2570,.F.);
#3479=ORIENTED_EDGE('',*,*,#2571,.F.);
#3480=ORIENTED_EDGE('',*,*,#2572,.F.);
#3481=ORIENTED_EDGE('',*,*,#2573,.F.);
#3482=ORIENTED_EDGE('',*,*,#2574,.F.);
#3483=ORIENTED_EDGE('',*,*,#2568,.F.);
#3484=ORIENTED_EDGE('',*,*,#2564,.T.);
#3485=ORIENTED_EDGE('',*,*,#2575,.T.);
#3486=ORIENTED_EDGE('',*,*,#2573,.T.);
#3487=ORIENTED_EDGE('',*,*,#2576,.F.);
#3488=ORIENTED_EDGE('',*,*,#2563,.T.);
#3489=ORIENTED_EDGE('',*,*,#2577,.T.);
#3490=ORIENTED_EDGE('',*,*,#2574,.T.);
#3491=ORIENTED_EDGE('',*,*,#2575,.F.);
#3492=ORIENTED_EDGE('',*,*,#2560,.T.);
#3493=ORIENTED_EDGE('',*,*,#2578,.T.);
#3494=ORIENTED_EDGE('',*,*,#2569,.T.);
#3495=ORIENTED_EDGE('',*,*,#2577,.F.);
#3496=ORIENTED_EDGE('',*,*,#2579,.F.);
#3497=ORIENTED_EDGE('',*,*,#2580,.T.);
#3498=ORIENTED_EDGE('',*,*,#2581,.T.);
#3499=ORIENTED_EDGE('',*,*,#2580,.F.);
#3500=ORIENTED_EDGE('',*,*,#2559,.T.);
#3501=ORIENTED_EDGE('',*,*,#2582,.T.);
#3502=ORIENTED_EDGE('',*,*,#2570,.T.);
#3503=ORIENTED_EDGE('',*,*,#2578,.F.);
#3504=ORIENTED_EDGE('',*,*,#2565,.T.);
#3505=ORIENTED_EDGE('',*,*,#2576,.T.);
#3506=ORIENTED_EDGE('',*,*,#2572,.T.);
#3507=ORIENTED_EDGE('',*,*,#2583,.F.);
#3508=ORIENTED_EDGE('',*,*,#2566,.T.);
#3509=ORIENTED_EDGE('',*,*,#2583,.T.);
#3510=ORIENTED_EDGE('',*,*,#2571,.T.);
#3511=ORIENTED_EDGE('',*,*,#2582,.F.);
#3512=ORIENTED_EDGE('',*,*,#2567,.T.);
#3513=ORIENTED_EDGE('',*,*,#2579,.T.);
#3514=ORIENTED_EDGE('',*,*,#2562,.T.);
#3515=ORIENTED_EDGE('',*,*,#2581,.F.);
#3516=ORIENTED_EDGE('',*,*,#2584,.F.);
#3517=ORIENTED_EDGE('',*,*,#2585,.T.);
#3518=ORIENTED_EDGE('',*,*,#2586,.F.);
#3519=ORIENTED_EDGE('',*,*,#2585,.F.);
#3520=ORIENTED_EDGE('',*,*,#2587,.F.);
#3521=ORIENTED_EDGE('',*,*,#2588,.T.);
#3522=ORIENTED_EDGE('',*,*,#2589,.F.);
#3523=ORIENTED_EDGE('',*,*,#2588,.F.);
#3524=ORIENTED_EDGE('',*,*,#2590,.F.);
#3525=ORIENTED_EDGE('',*,*,#2591,.T.);
#3526=ORIENTED_EDGE('',*,*,#2592,.F.);
#3527=ORIENTED_EDGE('',*,*,#2591,.F.);
#3528=ORIENTED_EDGE('',*,*,#2593,.F.);
#3529=ORIENTED_EDGE('',*,*,#2594,.T.);
#3530=ORIENTED_EDGE('',*,*,#2595,.F.);
#3531=ORIENTED_EDGE('',*,*,#2594,.F.);
#3532=ORIENTED_EDGE('',*,*,#2596,.T.);
#3533=ORIENTED_EDGE('',*,*,#2597,.T.);
#3534=ORIENTED_EDGE('',*,*,#2598,.F.);
#3535=ORIENTED_EDGE('',*,*,#2599,.F.);
#3536=ORIENTED_EDGE('',*,*,#2600,.T.);
#3537=ORIENTED_EDGE('',*,*,#2599,.T.);
#3538=ORIENTED_EDGE('',*,*,#2601,.F.);
#3539=ORIENTED_EDGE('',*,*,#2602,.F.);
#3540=ORIENTED_EDGE('',*,*,#2603,.T.);
#3541=ORIENTED_EDGE('',*,*,#2602,.T.);
#3542=ORIENTED_EDGE('',*,*,#2604,.F.);
#3543=ORIENTED_EDGE('',*,*,#2605,.F.);
#3544=ORIENTED_EDGE('',*,*,#2606,.T.);
#3545=ORIENTED_EDGE('',*,*,#2605,.T.);
#3546=ORIENTED_EDGE('',*,*,#2607,.F.);
#3547=ORIENTED_EDGE('',*,*,#2597,.F.);
#3548=ORIENTED_EDGE('',*,*,#2607,.T.);
#3549=ORIENTED_EDGE('',*,*,#2604,.T.);
#3550=ORIENTED_EDGE('',*,*,#2601,.T.);
#3551=ORIENTED_EDGE('',*,*,#2598,.T.);
#3552=ORIENTED_EDGE('',*,*,#2586,.T.);
#3553=ORIENTED_EDGE('',*,*,#2589,.T.);
#3554=ORIENTED_EDGE('',*,*,#2592,.T.);
#3555=ORIENTED_EDGE('',*,*,#2595,.T.);
#3556=ORIENTED_EDGE('',*,*,#2606,.F.);
#3557=ORIENTED_EDGE('',*,*,#2596,.F.);
#3558=ORIENTED_EDGE('',*,*,#2600,.F.);
#3559=ORIENTED_EDGE('',*,*,#2603,.F.);
#3560=ORIENTED_EDGE('',*,*,#2584,.T.);
#3561=ORIENTED_EDGE('',*,*,#2587,.T.);
#3562=ORIENTED_EDGE('',*,*,#2590,.T.);
#3563=ORIENTED_EDGE('',*,*,#2593,.T.);
#3564=ORIENTED_EDGE('',*,*,#2608,.F.);
#3565=ORIENTED_EDGE('',*,*,#2609,.T.);
#3566=ORIENTED_EDGE('',*,*,#2610,.F.);
#3567=ORIENTED_EDGE('',*,*,#2609,.F.);
#3568=ORIENTED_EDGE('',*,*,#2608,.T.);
#3569=ORIENTED_EDGE('',*,*,#2611,.F.);
#3570=ORIENTED_EDGE('',*,*,#2612,.T.);
#3571=ORIENTED_EDGE('',*,*,#2613,.F.);
#3572=ORIENTED_EDGE('',*,*,#2612,.F.);
#3573=ORIENTED_EDGE('',*,*,#2611,.T.);
#3574=ORIENTED_EDGE('',*,*,#2614,.F.);
#3575=ORIENTED_EDGE('',*,*,#2615,.F.);
#3576=ORIENTED_EDGE('',*,*,#2616,.F.);
#3577=ORIENTED_EDGE('',*,*,#2617,.F.);
#3578=ORIENTED_EDGE('',*,*,#2615,.T.);
#3579=ORIENTED_EDGE('',*,*,#2618,.T.);
#3580=ORIENTED_EDGE('',*,*,#2619,.F.);
#3581=ORIENTED_EDGE('',*,*,#2620,.F.);
#3582=ORIENTED_EDGE('',*,*,#2614,.T.);
#3583=ORIENTED_EDGE('',*,*,#2621,.T.);
#3584=ORIENTED_EDGE('',*,*,#2622,.F.);
#3585=ORIENTED_EDGE('',*,*,#2618,.F.);
#3586=ORIENTED_EDGE('',*,*,#2616,.T.);
#3587=ORIENTED_EDGE('',*,*,#2620,.T.);
#3588=ORIENTED_EDGE('',*,*,#2623,.F.);
#3589=ORIENTED_EDGE('',*,*,#2624,.F.);
#3590=ORIENTED_EDGE('',*,*,#2617,.T.);
#3591=ORIENTED_EDGE('',*,*,#2624,.T.);
#3592=ORIENTED_EDGE('',*,*,#2625,.F.);
#3593=ORIENTED_EDGE('',*,*,#2621,.F.);
#3594=ORIENTED_EDGE('',*,*,#2625,.T.);
#3595=ORIENTED_EDGE('',*,*,#2623,.T.);
#3596=ORIENTED_EDGE('',*,*,#2619,.T.);
#3597=ORIENTED_EDGE('',*,*,#2622,.T.);
#3598=ORIENTED_EDGE('',*,*,#2610,.T.);
#3599=ORIENTED_EDGE('',*,*,#2613,.T.);
#3600=ORIENTED_EDGE('',*,*,#2626,.F.);
#3601=ORIENTED_EDGE('',*,*,#2627,.T.);
#3602=ORIENTED_EDGE('',*,*,#2628,.T.);
#3603=ORIENTED_EDGE('',*,*,#2627,.F.);
#3604=ORIENTED_EDGE('',*,*,#2626,.T.);
#3605=ORIENTED_EDGE('',*,*,#2628,.F.);
#3606=ORIENTED_EDGE('',*,*,#2629,.F.);
#3607=ORIENTED_EDGE('',*,*,#2630,.T.);
#3608=ORIENTED_EDGE('',*,*,#2631,.T.);
#3609=ORIENTED_EDGE('',*,*,#2630,.F.);
#3610=ORIENTED_EDGE('',*,*,#2629,.T.);
#3611=ORIENTED_EDGE('',*,*,#2631,.F.);
#3612=ORIENTED_EDGE('',*,*,#2632,.T.);
#3613=ORIENTED_EDGE('',*,*,#2633,.T.);
#3614=ORIENTED_EDGE('',*,*,#2634,.T.);
#3615=ORIENTED_EDGE('',*,*,#2635,.F.);
#3616=ORIENTED_EDGE('',*,*,#2636,.T.);
#3617=ORIENTED_EDGE('',*,*,#2637,.T.);
#3618=ORIENTED_EDGE('',*,*,#2638,.T.);
#3619=ORIENTED_EDGE('',*,*,#2633,.F.);
#3620=ORIENTED_EDGE('',*,*,#2639,.T.);
#3621=ORIENTED_EDGE('',*,*,#2640,.T.);
#3622=ORIENTED_EDGE('',*,*,#2641,.T.);
#3623=ORIENTED_EDGE('',*,*,#2637,.F.);
#3624=ORIENTED_EDGE('',*,*,#2642,.T.);
#3625=ORIENTED_EDGE('',*,*,#2643,.T.);
#3626=ORIENTED_EDGE('',*,*,#2644,.T.);
#3627=ORIENTED_EDGE('',*,*,#2640,.F.);
#3628=ORIENTED_EDGE('',*,*,#2645,.T.);
#3629=ORIENTED_EDGE('',*,*,#2646,.T.);
#3630=ORIENTED_EDGE('',*,*,#2647,.T.);
#3631=ORIENTED_EDGE('',*,*,#2643,.F.);
#3632=ORIENTED_EDGE('',*,*,#2648,.T.);
#3633=ORIENTED_EDGE('',*,*,#2635,.T.);
#3634=ORIENTED_EDGE('',*,*,#2649,.T.);
#3635=ORIENTED_EDGE('',*,*,#2646,.F.);
#3636=ORIENTED_EDGE('',*,*,#2648,.F.);
#3637=ORIENTED_EDGE('',*,*,#2645,.F.);
#3638=ORIENTED_EDGE('',*,*,#2642,.F.);
#3639=ORIENTED_EDGE('',*,*,#2639,.F.);
#3640=ORIENTED_EDGE('',*,*,#2636,.F.);
#3641=ORIENTED_EDGE('',*,*,#2632,.F.);
#3642=ORIENTED_EDGE('',*,*,#2649,.F.);
#3643=ORIENTED_EDGE('',*,*,#2634,.F.);
#3644=ORIENTED_EDGE('',*,*,#2638,.F.);
#3645=ORIENTED_EDGE('',*,*,#2641,.F.);
#3646=ORIENTED_EDGE('',*,*,#2644,.F.);
#3647=ORIENTED_EDGE('',*,*,#2647,.F.);
#3648=ORIENTED_EDGE('',*,*,#2650,.F.);
#3649=ORIENTED_EDGE('',*,*,#2651,.F.);
#3650=ORIENTED_EDGE('',*,*,#2652,.F.);
#3651=ORIENTED_EDGE('',*,*,#2653,.T.);
#3652=ORIENTED_EDGE('',*,*,#2651,.T.);
#3653=ORIENTED_EDGE('',*,*,#2653,.F.);
#3654=ORIENTED_EDGE('',*,*,#2654,.F.);
#3655=ORIENTED_EDGE('',*,*,#2655,.T.);
#3656=ORIENTED_EDGE('',*,*,#2652,.T.);
#3657=ORIENTED_EDGE('',*,*,#2655,.F.);
#3658=ORIENTED_EDGE('',*,*,#2656,.F.);
#3659=ORIENTED_EDGE('',*,*,#2657,.T.);
#3660=ORIENTED_EDGE('',*,*,#2654,.T.);
#3661=ORIENTED_EDGE('',*,*,#2657,.F.);
#3662=ORIENTED_EDGE('',*,*,#2656,.T.);
#3663=ORIENTED_EDGE('',*,*,#2658,.F.);
#3664=ORIENTED_EDGE('',*,*,#2659,.F.);
#3665=ORIENTED_EDGE('',*,*,#2660,.T.);
#3666=ORIENTED_EDGE('',*,*,#2658,.T.);
#3667=ORIENTED_EDGE('',*,*,#2660,.F.);
#3668=ORIENTED_EDGE('',*,*,#2650,.T.);
#3669=ORIENTED_EDGE('',*,*,#2661,.T.);
#3670=ORIENTED_EDGE('',*,*,#2659,.T.);
#3671=ORIENTED_EDGE('',*,*,#2661,.F.);
#3672=ORIENTED_EDGE('',*,*,#2662,.F.);
#3673=ORIENTED_EDGE('',*,*,#2663,.T.);
#3674=ORIENTED_EDGE('',*,*,#2664,.T.);
#3675=ORIENTED_EDGE('',*,*,#2663,.F.);
#3676=ORIENTED_EDGE('',*,*,#2665,.F.);
#3677=ORIENTED_EDGE('',*,*,#2666,.T.);
#3678=ORIENTED_EDGE('',*,*,#2667,.T.);
#3679=ORIENTED_EDGE('',*,*,#2666,.F.);
#3680=ORIENTED_EDGE('',*,*,#2665,.T.);
#3681=ORIENTED_EDGE('',*,*,#2662,.T.);
#3682=ORIENTED_EDGE('',*,*,#2667,.F.);
#3683=ORIENTED_EDGE('',*,*,#2664,.F.);
#3684=ORIENTED_EDGE('',*,*,#2668,.F.);
#3685=ORIENTED_EDGE('',*,*,#2669,.F.);
#3686=ORIENTED_EDGE('',*,*,#2670,.T.);
#3687=ORIENTED_EDGE('',*,*,#2671,.F.);
#3688=ORIENTED_EDGE('',*,*,#2670,.F.);
#3689=ORIENTED_EDGE('',*,*,#2672,.F.);
#3690=ORIENTED_EDGE('',*,*,#2673,.F.);
#3691=ORIENTED_EDGE('',*,*,#2674,.F.);
#3692=ORIENTED_EDGE('',*,*,#2675,.F.);
#3693=ORIENTED_EDGE('',*,*,#2676,.F.);
#3694=ORIENTED_EDGE('',*,*,#2677,.T.);
#3695=ORIENTED_EDGE('',*,*,#2678,.F.);
#3696=ORIENTED_EDGE('',*,*,#2679,.F.);
#3697=ORIENTED_EDGE('',*,*,#2680,.F.);
#3698=ORIENTED_EDGE('',*,*,#2681,.F.);
#3699=ORIENTED_EDGE('',*,*,#2682,.F.);
#3700=ORIENTED_EDGE('',*,*,#2683,.F.);
#3701=ORIENTED_EDGE('',*,*,#2677,.F.);
#3702=ORIENTED_EDGE('',*,*,#2673,.T.);
#3703=ORIENTED_EDGE('',*,*,#2684,.T.);
#3704=ORIENTED_EDGE('',*,*,#2682,.T.);
#3705=ORIENTED_EDGE('',*,*,#2685,.F.);
#3706=ORIENTED_EDGE('',*,*,#2672,.T.);
#3707=ORIENTED_EDGE('',*,*,#2686,.T.);
#3708=ORIENTED_EDGE('',*,*,#2683,.T.);
#3709=ORIENTED_EDGE('',*,*,#2684,.F.);
#3710=ORIENTED_EDGE('',*,*,#2669,.T.);
#3711=ORIENTED_EDGE('',*,*,#2687,.T.);
#3712=ORIENTED_EDGE('',*,*,#2678,.T.);
#3713=ORIENTED_EDGE('',*,*,#2686,.F.);
#3714=ORIENTED_EDGE('',*,*,#2688,.F.);
#3715=ORIENTED_EDGE('',*,*,#2689,.T.);
#3716=ORIENTED_EDGE('',*,*,#2690,.T.);
#3717=ORIENTED_EDGE('',*,*,#2689,.F.);
#3718=ORIENTED_EDGE('',*,*,#2668,.T.);
#3719=ORIENTED_EDGE('',*,*,#2691,.T.);
#3720=ORIENTED_EDGE('',*,*,#2679,.T.);
#3721=ORIENTED_EDGE('',*,*,#2687,.F.);
#3722=ORIENTED_EDGE('',*,*,#2674,.T.);
#3723=ORIENTED_EDGE('',*,*,#2685,.T.);
#3724=ORIENTED_EDGE('',*,*,#2681,.T.);
#3725=ORIENTED_EDGE('',*,*,#2692,.F.);
#3726=ORIENTED_EDGE('',*,*,#2675,.T.);
#3727=ORIENTED_EDGE('',*,*,#2692,.T.);
#3728=ORIENTED_EDGE('',*,*,#2680,.T.);
#3729=ORIENTED_EDGE('',*,*,#2691,.F.);
#3730=ORIENTED_EDGE('',*,*,#2676,.T.);
#3731=ORIENTED_EDGE('',*,*,#2688,.T.);
#3732=ORIENTED_EDGE('',*,*,#2671,.T.);
#3733=ORIENTED_EDGE('',*,*,#2690,.F.);
#3734=ORIENTED_EDGE('',*,*,#2693,.F.);
#3735=ORIENTED_EDGE('',*,*,#2694,.T.);
#3736=ORIENTED_EDGE('',*,*,#2695,.T.);
#3737=ORIENTED_EDGE('',*,*,#2694,.F.);
#3738=ORIENTED_EDGE('',*,*,#2693,.T.);
#3739=ORIENTED_EDGE('',*,*,#2695,.F.);
#3740=PLANE('',#4407);
#3741=PLANE('',#4408);
#3742=PLANE('',#4409);
#3743=PLANE('',#4410);
#3744=PLANE('',#4411);
#3745=PLANE('',#4412);
#3746=PLANE('',#4413);
#3747=PLANE('',#4414);
#3748=PLANE('',#4415);
#3749=PLANE('',#4416);
#3750=PLANE('',#4453);
#3751=PLANE('',#4454);
#3752=PLANE('',#4455);
#3753=PLANE('',#4456);
#3754=PLANE('',#4457);
#3755=PLANE('',#4458);
#3756=PLANE('',#4466);
#3757=PLANE('',#4467);
#3758=PLANE('',#4468);
#3759=PLANE('',#4469);
#3760=PLANE('',#4470);
#3761=PLANE('',#4471);
#3762=PLANE('',#4473);
#3763=PLANE('',#4474);
#3764=PLANE('',#4475);
#3765=PLANE('',#4476);
#3766=PLANE('',#4477);
#3767=PLANE('',#4478);
#3768=PLANE('',#4486);
#3769=PLANE('',#4487);
#3770=PLANE('',#4488);
#3771=PLANE('',#4489);
#3772=PLANE('',#4490);
#3773=PLANE('',#4491);
#3774=PLANE('',#4493);
#3775=PLANE('',#4494);
#3776=PLANE('',#4495);
#3777=PLANE('',#4496);
#3778=PLANE('',#4497);
#3779=PLANE('',#4498);
#3780=PLANE('',#4507);
#3781=PLANE('',#4508);
#3782=PLANE('',#4509);
#3783=PLANE('',#4510);
#3784=PLANE('',#4511);
#3785=PLANE('',#4515);
#3786=PLANE('',#4521);
#3787=PLANE('',#4523);
#3788=PLANE('',#4524);
#3789=PLANE('',#4525);
#3790=PLANE('',#4526);
#3791=PLANE('',#4531);
#3792=PLANE('',#4532);
#3793=PLANE('',#4533);
#3794=PLANE('',#4534);
#3795=PLANE('',#4535);
#3796=PLANE('',#4536);
#3797=PLANE('',#4537);
#3798=PLANE('',#4546);
#3799=PLANE('',#4547);
#3800=PLANE('',#4548);
#3801=PLANE('',#4549);
#3802=PLANE('',#4550);
#3803=PLANE('',#4554);
#3804=PLANE('',#4560);
#3805=PLANE('',#4562);
#3806=PLANE('',#4563);
#3807=PLANE('',#4564);
#3808=PLANE('',#4565);
#3809=PLANE('',#4570);
#3810=PLANE('',#4571);
#3811=PLANE('',#4572);
#3812=PLANE('',#4573);
#3813=PLANE('',#4574);
#3814=PLANE('',#4575);
#3815=PLANE('',#4576);
#3816=PLANE('',#4587);
#3817=PLANE('',#4595);
#3818=PLANE('',#4597);
#3819=PLANE('',#4598);
#3820=PLANE('',#4599);
#3821=PLANE('',#4604);
#3822=PLANE('',#4605);
#3823=PLANE('',#4606);
#3824=PLANE('',#4607);
#3825=PLANE('',#4608);
#3826=PLANE('',#4610);
#3827=PLANE('',#4611);
#3828=PLANE('',#4612);
#3829=PLANE('',#4613);
#3830=PLANE('',#4614);
#3831=PLANE('',#4615);
#3832=PLANE('',#4616);
#3833=PLANE('',#4617);
#3834=PLANE('',#4618);
#3835=PLANE('',#4619);
#3836=PLANE('',#4621);
#3837=PLANE('',#4629);
#3838=PLANE('',#4637);
#3839=PLANE('',#4638);
#3840=PLANE('',#4639);
#3841=PLANE('',#4640);
#3842=PLANE('',#4641);
#3843=PLANE('',#4642);
#3844=PLANE('',#4643);
#3845=PLANE('',#4644);
#3846=PLANE('',#4645);
#3847=PLANE('',#4647);
#3848=PLANE('',#4655);
#3849=PLANE('',#4663);
#3850=PLANE('',#4664);
#3851=PLANE('',#4665);
#3852=PLANE('',#4666);
#3853=PLANE('',#4667);
#3854=PLANE('',#4668);
#3855=PLANE('',#4669);
#3856=PLANE('',#4670);
#3857=PLANE('',#4671);
#3858=PLANE('',#4679);
#3859=PLANE('',#4680);
#3860=PLANE('',#4686);
#3861=PLANE('',#4687);
#3862=PLANE('',#4688);
#3863=PLANE('',#4692);
#3864=PLANE('',#4693);
#3865=PLANE('',#4694);
#3866=PLANE('',#4695);
#3867=PLANE('',#4696);
#3868=PLANE('',#4734);
#3869=PLANE('',#4735);
#3870=PLANE('',#4736);
#3871=PLANE('',#4737);
#3872=PLANE('',#4738);
#3873=PLANE('',#4739);
#3874=PLANE('',#4744);
#3875=PLANE('',#4748);
#3876=PLANE('',#4752);
#3877=PLANE('',#4753);
#3878=PLANE('',#4754);
#3879=PLANE('',#4755);
#3880=PLANE('',#4756);
#3881=PLANE('',#4761);
#3882=PLANE('',#4762);
#3883=PLANE('',#4767);
#3884=PLANE('',#4768);
#3885=PLANE('',#4770);
#3886=PLANE('',#4771);
#3887=PLANE('',#4772);
#3888=PLANE('',#4773);
#3889=PLANE('',#4774);
#3890=PLANE('',#4775);
#3891=PLANE('',#4776);
#3892=PLANE('',#4777);
#3893=PLANE('',#4778);
#3894=PLANE('',#4780);
#3895=PLANE('',#4788);
#3896=PLANE('',#4800);
#3897=PLANE('',#4801);
#3898=PLANE('',#4807);
#3899=PLANE('',#4808);
#3900=PLANE('',#4809);
#3901=PLANE('',#4813);
#3902=PLANE('',#4814);
#3903=PLANE('',#4815);
#3904=PLANE('',#4816);
#3905=PLANE('',#4817);
#3906=PLANE('',#4837);
#3907=PLANE('',#4838);
#3908=ADVANCED_FACE('',(#562),#3740,.F.);
#3909=ADVANCED_FACE('',(#563),#3741,.F.);
#3910=ADVANCED_FACE('',(#564),#3742,.F.);
#3911=ADVANCED_FACE('',(#565),#3743,.F.);
#3912=ADVANCED_FACE('',(#566),#3744,.T.);
#3913=ADVANCED_FACE('',(#567),#3745,.F.);
#3914=ADVANCED_FACE('',(#568),#3746,.F.);
#3915=ADVANCED_FACE('',(#569),#3747,.F.);
#3916=ADVANCED_FACE('',(#570),#3748,.F.);
#3917=ADVANCED_FACE('',(#571),#3749,.T.);
#3918=ADVANCED_FACE('',(#572),#505,.F.);
#3919=ADVANCED_FACE('',(#573),#506,.F.);
#3920=ADVANCED_FACE('',(#574),#507,.F.);
#3921=ADVANCED_FACE('',(#575),#508,.F.);
#3922=ADVANCED_FACE('',(#576),#509,.F.);
#3923=ADVANCED_FACE('',(#577),#510,.F.);
#3924=ADVANCED_FACE('',(#578),#511,.F.);
#3925=ADVANCED_FACE('',(#579),#512,.F.);
#3926=ADVANCED_FACE('',(#580),#513,.F.);
#3927=ADVANCED_FACE('',(#581),#514,.F.);
#3928=ADVANCED_FACE('',(#582),#515,.F.);
#3929=ADVANCED_FACE('',(#583),#516,.F.);
#3930=ADVANCED_FACE('',(#584),#3750,.T.);
#3931=ADVANCED_FACE('',(#585),#3751,.T.);
#3932=ADVANCED_FACE('',(#586),#3752,.T.);
#3933=ADVANCED_FACE('',(#587),#3753,.T.);
#3934=ADVANCED_FACE('',(#588,#305,#306,#307,#308,#309,#310,#311,#312,#313,
#314,#315,#316,#317,#318),#3754,.T.);
#3935=ADVANCED_FACE('',(#589,#319,#320,#321,#322,#323,#324,#325,#326,#327,
#328,#329,#330),#3755,.F.);
#3936=ADVANCED_FACE('',(#590),#517,.F.);
#3937=ADVANCED_FACE('',(#591),#518,.F.);
#3938=ADVANCED_FACE('',(#592),#3756,.T.);
#3939=ADVANCED_FACE('',(#593),#3757,.T.);
#3940=ADVANCED_FACE('',(#594),#3758,.T.);
#3941=ADVANCED_FACE('',(#595),#3759,.T.);
#3942=ADVANCED_FACE('',(#596,#331,#332),#3760,.T.);
#3943=ADVANCED_FACE('',(#597,#333,#334),#3761,.F.);
#3944=ADVANCED_FACE('',(#598),#3762,.T.);
#3945=ADVANCED_FACE('',(#599),#3763,.T.);
#3946=ADVANCED_FACE('',(#600),#3764,.T.);
#3947=ADVANCED_FACE('',(#601),#3765,.T.);
#3948=ADVANCED_FACE('',(#602),#3766,.T.);
#3949=ADVANCED_FACE('',(#603),#3767,.F.);
#3950=ADVANCED_FACE('',(#604),#519,.F.);
#3951=ADVANCED_FACE('',(#605),#520,.F.);
#3952=ADVANCED_FACE('',(#606),#3768,.T.);
#3953=ADVANCED_FACE('',(#607),#3769,.T.);
#3954=ADVANCED_FACE('',(#608),#3770,.T.);
#3955=ADVANCED_FACE('',(#609),#3771,.T.);
#3956=ADVANCED_FACE('',(#610,#335,#336),#3772,.T.);
#3957=ADVANCED_FACE('',(#611,#337,#338),#3773,.F.);
#3958=ADVANCED_FACE('',(#612),#3774,.T.);
#3959=ADVANCED_FACE('',(#613),#3775,.T.);
#3960=ADVANCED_FACE('',(#614),#3776,.T.);
#3961=ADVANCED_FACE('',(#615),#3777,.T.);
#3962=ADVANCED_FACE('',(#616),#3778,.T.);
#3963=ADVANCED_FACE('',(#617),#3779,.F.);
#3964=ADVANCED_FACE('',(#618),#521,.F.);
#3965=ADVANCED_FACE('',(#619),#522,.F.);
#3966=ADVANCED_FACE('',(#620),#3780,.F.);
#3967=ADVANCED_FACE('',(#621),#3781,.F.);
#3968=ADVANCED_FACE('',(#622),#3782,.F.);
#3969=ADVANCED_FACE('',(#623),#3783,.F.);
#3970=ADVANCED_FACE('',(#624),#3784,.F.);
#3971=ADVANCED_FACE('',(#625),#523,.F.);
#3972=ADVANCED_FACE('',(#626,#339),#3785,.T.);
#3973=ADVANCED_FACE('',(#627),#524,.F.);
#3974=ADVANCED_FACE('',(#628,#340),#3786,.T.);
#3975=ADVANCED_FACE('',(#629),#3787,.F.);
#3976=ADVANCED_FACE('',(#630),#3788,.T.);
#3977=ADVANCED_FACE('',(#631),#3789,.F.);
#3978=ADVANCED_FACE('',(#632),#3790,.T.);
#3979=ADVANCED_FACE('',(#633),#525,.F.);
#3980=ADVANCED_FACE('',(#634),#526,.F.);
#3981=ADVANCED_FACE('',(#635),#3791,.T.);
#3982=ADVANCED_FACE('',(#636),#3792,.T.);
#3983=ADVANCED_FACE('',(#637),#3793,.T.);
#3984=ADVANCED_FACE('',(#638),#3794,.T.);
#3985=ADVANCED_FACE('',(#639),#3795,.T.);
#3986=ADVANCED_FACE('',(#640),#3796,.T.);
#3987=ADVANCED_FACE('',(#641,#341,#342,#343),#3797,.F.);
#3988=ADVANCED_FACE('',(#642),#527,.F.);
#3989=ADVANCED_FACE('',(#643),#528,.F.);
#3990=ADVANCED_FACE('',(#644),#3798,.F.);
#3991=ADVANCED_FACE('',(#645),#3799,.F.);
#3992=ADVANCED_FACE('',(#646),#3800,.F.);
#3993=ADVANCED_FACE('',(#647),#3801,.F.);
#3994=ADVANCED_FACE('',(#648),#3802,.F.);
#3995=ADVANCED_FACE('',(#649),#529,.F.);
#3996=ADVANCED_FACE('',(#650,#344),#3803,.T.);
#3997=ADVANCED_FACE('',(#651),#530,.F.);
#3998=ADVANCED_FACE('',(#652,#345),#3804,.T.);
#3999=ADVANCED_FACE('',(#653),#3805,.F.);
#4000=ADVANCED_FACE('',(#654),#3806,.T.);
#4001=ADVANCED_FACE('',(#655),#3807,.F.);
#4002=ADVANCED_FACE('',(#656),#3808,.T.);
#4003=ADVANCED_FACE('',(#657),#531,.F.);
#4004=ADVANCED_FACE('',(#658),#532,.F.);
#4005=ADVANCED_FACE('',(#659),#3809,.T.);
#4006=ADVANCED_FACE('',(#660),#3810,.T.);
#4007=ADVANCED_FACE('',(#661),#3811,.T.);
#4008=ADVANCED_FACE('',(#662),#3812,.T.);
#4009=ADVANCED_FACE('',(#663),#3813,.T.);
#4010=ADVANCED_FACE('',(#664),#3814,.T.);
#4011=ADVANCED_FACE('',(#665,#346,#347,#348),#3815,.F.);
#4012=ADVANCED_FACE('',(#666),#533,.F.);
#4013=ADVANCED_FACE('',(#667),#534,.F.);
#4014=ADVANCED_FACE('',(#668),#535,.F.);
#4015=ADVANCED_FACE('',(#669,#349),#3816,.T.);
#4016=ADVANCED_FACE('',(#670),#536,.F.);
#4017=ADVANCED_FACE('',(#671),#537,.F.);
#4018=ADVANCED_FACE('',(#672,#350),#3817,.T.);
#4019=ADVANCED_FACE('',(#673),#3818,.T.);
#4020=ADVANCED_FACE('',(#674),#3819,.T.);
#4021=ADVANCED_FACE('',(#675),#3820,.T.);
#4022=ADVANCED_FACE('',(#676),#538,.F.);
#4023=ADVANCED_FACE('',(#677),#539,.F.);
#4024=ADVANCED_FACE('',(#678),#3821,.T.);
#4025=ADVANCED_FACE('',(#679,#351),#3822,.T.);
#4026=ADVANCED_FACE('',(#680),#3823,.T.);
#4027=ADVANCED_FACE('',(#681,#352),#3824,.T.);
#4028=ADVANCED_FACE('',(#682,#353,#354),#3825,.F.);
#4029=ADVANCED_FACE('',(#683),#3826,.F.);
#4030=ADVANCED_FACE('',(#684),#3827,.T.);
#4031=ADVANCED_FACE('',(#685),#3828,.T.);
#4032=ADVANCED_FACE('',(#686),#3829,.T.);
#4033=ADVANCED_FACE('',(#687),#3830,.T.);
#4034=ADVANCED_FACE('',(#688),#3831,.T.);
#4035=ADVANCED_FACE('',(#689),#3832,.F.);
#4036=ADVANCED_FACE('',(#690),#3833,.T.);
#4037=ADVANCED_FACE('',(#691),#3834,.T.);
#4038=ADVANCED_FACE('',(#692),#3835,.T.);
#4039=ADVANCED_FACE('',(#693),#3836,.T.);
#4040=ADVANCED_FACE('',(#694),#202,.T.);
#4041=ADVANCED_FACE('',(#695),#540,.T.);
#4042=ADVANCED_FACE('',(#696),#203,.T.);
#4043=ADVANCED_FACE('',(#697,#355),#3837,.T.);
#4044=ADVANCED_FACE('',(#698),#204,.T.);
#4045=ADVANCED_FACE('',(#699),#541,.T.);
#4046=ADVANCED_FACE('',(#700),#205,.T.);
#4047=ADVANCED_FACE('',(#701),#3838,.T.);
#4048=ADVANCED_FACE('',(#702),#3839,.F.);
#4049=ADVANCED_FACE('',(#703),#3840,.F.);
#4050=ADVANCED_FACE('',(#704),#3841,.F.);
#4051=ADVANCED_FACE('',(#705),#3842,.F.);
#4052=ADVANCED_FACE('',(#706),#3843,.F.);
#4053=ADVANCED_FACE('',(#707),#3844,.F.);
#4054=ADVANCED_FACE('',(#708),#3845,.F.);
#4055=ADVANCED_FACE('',(#709),#3846,.F.);
#4056=ADVANCED_FACE('',(#710),#3847,.T.);
#4057=ADVANCED_FACE('',(#711),#206,.T.);
#4058=ADVANCED_FACE('',(#712),#542,.T.);
#4059=ADVANCED_FACE('',(#713),#207,.T.);
#4060=ADVANCED_FACE('',(#714,#356),#3848,.T.);
#4061=ADVANCED_FACE('',(#715),#208,.T.);
#4062=ADVANCED_FACE('',(#716),#543,.T.);
#4063=ADVANCED_FACE('',(#717),#209,.T.);
#4064=ADVANCED_FACE('',(#718),#3849,.T.);
#4065=ADVANCED_FACE('',(#719),#3850,.F.);
#4066=ADVANCED_FACE('',(#720),#3851,.F.);
#4067=ADVANCED_FACE('',(#721),#3852,.F.);
#4068=ADVANCED_FACE('',(#722),#3853,.F.);
#4069=ADVANCED_FACE('',(#723),#3854,.F.);
#4070=ADVANCED_FACE('',(#724),#3855,.F.);
#4071=ADVANCED_FACE('',(#725),#3856,.F.);
#4072=ADVANCED_FACE('',(#726),#3857,.F.);
#4073=ADVANCED_FACE('',(#727),#544,.F.);
#4074=ADVANCED_FACE('',(#728),#545,.T.);
#4075=ADVANCED_FACE('',(#729,#357),#3858,.T.);
#4076=ADVANCED_FACE('',(#730,#358),#3859,.F.);
#4077=ADVANCED_FACE('',(#731),#210,.T.);
#4078=ADVANCED_FACE('',(#732),#211,.T.);
#4079=ADVANCED_FACE('',(#733),#3860,.T.);
#4080=ADVANCED_FACE('',(#734),#3861,.T.);
#4081=ADVANCED_FACE('',(#735),#3862,.T.);
#4082=ADVANCED_FACE('',(#736),#546,.F.);
#4083=ADVANCED_FACE('',(#737),#3863,.T.);
#4084=ADVANCED_FACE('',(#738),#3864,.T.);
#4085=ADVANCED_FACE('',(#739),#3865,.T.);
#4086=ADVANCED_FACE('',(#740,#359),#3866,.T.);
#4087=ADVANCED_FACE('',(#741,#360),#3867,.F.);
#4088=ADVANCED_FACE('',(#742),#547,.F.);
#4089=ADVANCED_FACE('',(#743),#548,.F.);
#4090=ADVANCED_FACE('',(#744),#549,.F.);
#4091=ADVANCED_FACE('',(#745),#550,.F.);
#4092=ADVANCED_FACE('',(#746),#3868,.T.);
#4093=ADVANCED_FACE('',(#747),#3869,.T.);
#4094=ADVANCED_FACE('',(#748),#3870,.T.);
#4095=ADVANCED_FACE('',(#749),#3871,.T.);
#4096=ADVANCED_FACE('',(#750,#361,#362,#363,#364),#3872,.T.);
#4097=ADVANCED_FACE('',(#751,#365,#366,#367,#368),#3873,.F.);
#4098=ADVANCED_FACE('',(#752),#551,.F.);
#4099=ADVANCED_FACE('',(#753),#3874,.T.);
#4100=ADVANCED_FACE('',(#754),#552,.F.);
#4101=ADVANCED_FACE('',(#755),#3875,.T.);
#4102=ADVANCED_FACE('',(#756),#553,.F.);
#4103=ADVANCED_FACE('',(#757),#3876,.T.);
#4104=ADVANCED_FACE('',(#758),#3877,.T.);
#4105=ADVANCED_FACE('',(#759),#3878,.T.);
#4106=ADVANCED_FACE('',(#760),#3879,.T.);
#4107=ADVANCED_FACE('',(#761,#369,#370),#3880,.T.);
#4108=ADVANCED_FACE('',(#762),#554,.T.);
#4109=ADVANCED_FACE('',(#763),#3881,.T.);
#4110=ADVANCED_FACE('',(#764),#3882,.F.);
#4111=ADVANCED_FACE('',(#765),#555,.T.);
#4112=ADVANCED_FACE('',(#766),#3883,.T.);
#4113=ADVANCED_FACE('',(#767),#3884,.F.);
#4114=ADVANCED_FACE('',(#768),#3885,.F.);
#4115=ADVANCED_FACE('',(#769),#3886,.F.);
#4116=ADVANCED_FACE('',(#770),#3887,.F.);
#4117=ADVANCED_FACE('',(#771),#3888,.F.);
#4118=ADVANCED_FACE('',(#772),#3889,.F.);
#4119=ADVANCED_FACE('',(#773),#3890,.F.);
#4120=ADVANCED_FACE('',(#774),#3891,.F.);
#4121=ADVANCED_FACE('',(#775),#3892,.F.);
#4122=ADVANCED_FACE('',(#776),#3893,.F.);
#4123=ADVANCED_FACE('',(#777),#3894,.T.);
#4124=ADVANCED_FACE('',(#778),#212,.T.);
#4125=ADVANCED_FACE('',(#779),#556,.T.);
#4126=ADVANCED_FACE('',(#780),#213,.T.);
#4127=ADVANCED_FACE('',(#781,#371),#3895,.T.);
#4128=ADVANCED_FACE('',(#782),#214,.T.);
#4129=ADVANCED_FACE('',(#783),#557,.T.);
#4130=ADVANCED_FACE('',(#784),#558,.F.);
#4131=ADVANCED_FACE('',(#785),#559,.T.);
#4132=ADVANCED_FACE('',(#786,#372),#3896,.T.);
#4133=ADVANCED_FACE('',(#787,#373),#3897,.F.);
#4134=ADVANCED_FACE('',(#788),#215,.T.);
#4135=ADVANCED_FACE('',(#789),#216,.T.);
#4136=ADVANCED_FACE('',(#790),#3898,.T.);
#4137=ADVANCED_FACE('',(#791),#3899,.T.);
#4138=ADVANCED_FACE('',(#792),#3900,.T.);
#4139=ADVANCED_FACE('',(#793),#560,.F.);
#4140=ADVANCED_FACE('',(#794),#3901,.T.);
#4141=ADVANCED_FACE('',(#795),#3902,.T.);
#4142=ADVANCED_FACE('',(#796),#3903,.T.);
#4143=ADVANCED_FACE('',(#797,#374),#3904,.T.);
#4144=ADVANCED_FACE('',(#798,#375),#3905,.F.);
#4145=ADVANCED_FACE('',(#799),#561,.T.);
#4146=ADVANCED_FACE('',(#800),#3906,.T.);
#4147=ADVANCED_FACE('',(#801),#3907,.F.);
#4148=CLOSED_SHELL('',(#3908,#3909,#3910,#3911,#3912,#3913,#3914,#3915,
#3916,#3917,#3918,#3919,#3920,#3921,#3922,#3923,#3924,#3925,#3926,#3927,
#3928,#3929,#3930,#3931,#3932,#3933,#3934,#3935));
#4149=CLOSED_SHELL('',(#3936,#3937,#3938,#3939,#3940,#3941,#3942,#3943));
#4150=CLOSED_SHELL('',(#3944,#3945,#3946,#3947,#3948,#3949));
#4151=CLOSED_SHELL('',(#3950,#3951,#3952,#3953,#3954,#3955,#3956,#3957));
#4152=CLOSED_SHELL('',(#3958,#3959,#3960,#3961,#3962,#3963));
#4153=CLOSED_SHELL('',(#3964,#3965,#3966,#3967,#3968,#3969,#3970,#3971,
#3972,#3973,#3974,#3975,#3976,#3977,#3978,#3979,#3980,#3981,#3982,#3983,
#3984,#3985,#3986,#3987));
#4154=CLOSED_SHELL('',(#3988,#3989,#3990,#3991,#3992,#3993,#3994,#3995,
#3996,#3997,#3998,#3999,#4000,#4001,#4002,#4003,#4004,#4005,#4006,#4007,
#4008,#4009,#4010,#4011));
#4155=CLOSED_SHELL('',(#4012,#4013,#4014,#4015,#4016,#4017,#4018,#4019,
#4020,#4021,#4022,#4023,#4024,#4025,#4026,#4027,#4028));
#4156=CLOSED_SHELL('',(#4029,#4030,#4031,#4032,#4033,#4034,#4035,#4036,
#4037,#4038));
#4157=CLOSED_SHELL('',(#4039,#4040,#4041,#4042,#4043,#4044,#4045,#4046,
#4047));
#4158=CLOSED_SHELL('',(#4048,#4049,#4050,#4051,#4052,#4053,#4054,#4055));
#4159=CLOSED_SHELL('',(#4056,#4057,#4058,#4059,#4060,#4061,#4062,#4063,
#4064));
#4160=CLOSED_SHELL('',(#4065,#4066,#4067,#4068,#4069,#4070,#4071,#4072));
#4161=CLOSED_SHELL('',(#4073,#4074,#4075,#4076));
#4162=CLOSED_SHELL('',(#4077,#4078,#4079,#4080,#4081,#4082,#4083,#4084,
#4085,#4086,#4087));
#4163=CLOSED_SHELL('',(#4088,#4089,#4090,#4091,#4092,#4093,#4094,#4095,
#4096,#4097));
#4164=CLOSED_SHELL('',(#4098,#4099,#4100,#4101,#4102,#4103,#4104,#4105,
#4106,#4107));
#4165=CLOSED_SHELL('',(#4108,#4109,#4110));
#4166=CLOSED_SHELL('',(#4111,#4112,#4113));
#4167=CLOSED_SHELL('',(#4114,#4115,#4116,#4117,#4118,#4119,#4120,#4121));
#4168=CLOSED_SHELL('',(#4122,#4123,#4124,#4125,#4126,#4127,#4128,#4129));
#4169=CLOSED_SHELL('',(#4130,#4131,#4132,#4133));
#4170=CLOSED_SHELL('',(#4134,#4135,#4136,#4137,#4138,#4139,#4140,#4141,
#4142,#4143,#4144));
#4171=CLOSED_SHELL('',(#4145,#4146,#4147));
#4172=DERIVED_UNIT_ELEMENT(#4214,1.);
#4173=DERIVED_UNIT_ELEMENT(#7346,-3.);
#4174=DERIVED_UNIT_ELEMENT(#4214,1.);
#4175=DERIVED_UNIT_ELEMENT(#7346,-3.);
#4176=DERIVED_UNIT_ELEMENT(#4214,1.);
#4177=DERIVED_UNIT_ELEMENT(#7346,-3.);
#4178=DERIVED_UNIT_ELEMENT(#4214,1.);
#4179=DERIVED_UNIT_ELEMENT(#7346,-3.);
#4180=DERIVED_UNIT_ELEMENT(#4214,1.);
#4181=DERIVED_UNIT_ELEMENT(#7346,-3.);
#4182=DERIVED_UNIT_ELEMENT(#4214,1.);
#4183=DERIVED_UNIT_ELEMENT(#7346,-3.);
#4184=DERIVED_UNIT_ELEMENT(#4214,1.);
#4185=DERIVED_UNIT_ELEMENT(#7346,-3.);
#4186=DERIVED_UNIT_ELEMENT(#4214,1.);
#4187=DERIVED_UNIT_ELEMENT(#7346,-3.);
#4188=DERIVED_UNIT_ELEMENT(#4214,1.);
#4189=DERIVED_UNIT_ELEMENT(#7346,-3.);
#4190=DERIVED_UNIT_ELEMENT(#4214,1.);
#4191=DERIVED_UNIT_ELEMENT(#7346,-3.);
#4192=DERIVED_UNIT_ELEMENT(#4214,1.);
#4193=DERIVED_UNIT_ELEMENT(#7346,-3.);
#4194=DERIVED_UNIT_ELEMENT(#4214,1.);
#4195=DERIVED_UNIT_ELEMENT(#7346,-3.);
#4196=DERIVED_UNIT_ELEMENT(#4214,1.);
#4197=DERIVED_UNIT_ELEMENT(#7346,-3.);
#4198=DERIVED_UNIT_ELEMENT(#4214,1.);
#4199=DERIVED_UNIT_ELEMENT(#7346,-3.);
#4200=DERIVED_UNIT_ELEMENT(#4214,1.);
#4201=DERIVED_UNIT_ELEMENT(#7346,-3.);
#4202=DERIVED_UNIT_ELEMENT(#4214,1.);
#4203=DERIVED_UNIT_ELEMENT(#7346,-3.);
#4204=DERIVED_UNIT_ELEMENT(#4214,1.);
#4205=DERIVED_UNIT_ELEMENT(#7346,-3.);
#4206=DERIVED_UNIT_ELEMENT(#4214,1.);
#4207=DERIVED_UNIT_ELEMENT(#7346,-3.);
#4208=DERIVED_UNIT_ELEMENT(#4214,1.);
#4209=DERIVED_UNIT_ELEMENT(#7346,-3.);
#4210=DERIVED_UNIT_ELEMENT(#4214,1.);
#4211=DERIVED_UNIT_ELEMENT(#7346,-3.);
#4212=DERIVED_UNIT_ELEMENT(#4214,1.);
#4213=DERIVED_UNIT_ELEMENT(#7346,-3.);
#4214=(
MASS_UNIT()
NAMED_UNIT(*)
SI_UNIT(.KILO.,.GRAM.)
);
#4215=DERIVED_UNIT((#4172,#4173));
#4216=DERIVED_UNIT((#4174,#4175));
#4217=DERIVED_UNIT((#4176,#4177));
#4218=DERIVED_UNIT((#4178,#4179));
#4219=DERIVED_UNIT((#4180,#4181));
#4220=DERIVED_UNIT((#4182,#4183));
#4221=DERIVED_UNIT((#4184,#4185));
#4222=DERIVED_UNIT((#4186,#4187));
#4223=DERIVED_UNIT((#4188,#4189));
#4224=DERIVED_UNIT((#4190,#4191));
#4225=DERIVED_UNIT((#4192,#4193));
#4226=DERIVED_UNIT((#4194,#4195));
#4227=DERIVED_UNIT((#4196,#4197));
#4228=DERIVED_UNIT((#4198,#4199));
#4229=DERIVED_UNIT((#4200,#4201));
#4230=DERIVED_UNIT((#4202,#4203));
#4231=DERIVED_UNIT((#4204,#4205));
#4232=DERIVED_UNIT((#4206,#4207));
#4233=DERIVED_UNIT((#4208,#4209));
#4234=DERIVED_UNIT((#4210,#4211));
#4235=DERIVED_UNIT((#4212,#4213));
#4236=MEASURE_REPRESENTATION_ITEM('density measure',
POSITIVE_RATIO_MEASURE(7850.),#4215);
#4237=MEASURE_REPRESENTATION_ITEM('density measure',
POSITIVE_RATIO_MEASURE(7850.),#4216);
#4238=MEASURE_REPRESENTATION_ITEM('density measure',
POSITIVE_RATIO_MEASURE(7850.),#4217);
#4239=MEASURE_REPRESENTATION_ITEM('density measure',
POSITIVE_RATIO_MEASURE(7850.),#4218);
#4240=MEASURE_REPRESENTATION_ITEM('density measure',
POSITIVE_RATIO_MEASURE(7850.),#4219);
#4241=MEASURE_REPRESENTATION_ITEM('density measure',
POSITIVE_RATIO_MEASURE(7850.),#4220);
#4242=MEASURE_REPRESENTATION_ITEM('density measure',
POSITIVE_RATIO_MEASURE(7850.),#4221);
#4243=MEASURE_REPRESENTATION_ITEM('density measure',
POSITIVE_RATIO_MEASURE(7850.),#4222);
#4244=MEASURE_REPRESENTATION_ITEM('density measure',
POSITIVE_RATIO_MEASURE(7850.),#4223);
#4245=MEASURE_REPRESENTATION_ITEM('density measure',
POSITIVE_RATIO_MEASURE(7850.),#4224);
#4246=MEASURE_REPRESENTATION_ITEM('density measure',
POSITIVE_RATIO_MEASURE(7850.),#4225);
#4247=MEASURE_REPRESENTATION_ITEM('density measure',
POSITIVE_RATIO_MEASURE(7850.),#4226);
#4248=MEASURE_REPRESENTATION_ITEM('density measure',
POSITIVE_RATIO_MEASURE(7850.),#4227);
#4249=MEASURE_REPRESENTATION_ITEM('density measure',
POSITIVE_RATIO_MEASURE(7850.),#4228);
#4250=MEASURE_REPRESENTATION_ITEM('density measure',
POSITIVE_RATIO_MEASURE(7850.),#4229);
#4251=MEASURE_REPRESENTATION_ITEM('density measure',
POSITIVE_RATIO_MEASURE(7850.),#4230);
#4252=MEASURE_REPRESENTATION_ITEM('density measure',
POSITIVE_RATIO_MEASURE(7850.),#4231);
#4253=MEASURE_REPRESENTATION_ITEM('density measure',
POSITIVE_RATIO_MEASURE(7850.),#4232);
#4254=MEASURE_REPRESENTATION_ITEM('density measure',
POSITIVE_RATIO_MEASURE(7850.),#4233);
#4255=MEASURE_REPRESENTATION_ITEM('density measure',
POSITIVE_RATIO_MEASURE(7850.),#4234);
#4256=MEASURE_REPRESENTATION_ITEM('density measure',
POSITIVE_RATIO_MEASURE(7850.),#4235);
#4257=PROPERTY_DEFINITION_REPRESENTATION(#4362,#4299);
#4258=PROPERTY_DEFINITION_REPRESENTATION(#4363,#4300);
#4259=PROPERTY_DEFINITION_REPRESENTATION(#4364,#4301);
#4260=PROPERTY_DEFINITION_REPRESENTATION(#4365,#4302);
#4261=PROPERTY_DEFINITION_REPRESENTATION(#4366,#4303);
#4262=PROPERTY_DEFINITION_REPRESENTATION(#4367,#4304);
#4263=PROPERTY_DEFINITION_REPRESENTATION(#4368,#4305);
#4264=PROPERTY_DEFINITION_REPRESENTATION(#4369,#4306);
#4265=PROPERTY_DEFINITION_REPRESENTATION(#4370,#4307);
#4266=PROPERTY_DEFINITION_REPRESENTATION(#4371,#4308);
#4267=PROPERTY_DEFINITION_REPRESENTATION(#4372,#4309);
#4268=PROPERTY_DEFINITION_REPRESENTATION(#4373,#4310);
#4269=PROPERTY_DEFINITION_REPRESENTATION(#4374,#4311);
#4270=PROPERTY_DEFINITION_REPRESENTATION(#4375,#4312);
#4271=PROPERTY_DEFINITION_REPRESENTATION(#4376,#4313);
#4272=PROPERTY_DEFINITION_REPRESENTATION(#4377,#4314);
#4273=PROPERTY_DEFINITION_REPRESENTATION(#4378,#4315);
#4274=PROPERTY_DEFINITION_REPRESENTATION(#4379,#4316);
#4275=PROPERTY_DEFINITION_REPRESENTATION(#4380,#4317);
#4276=PROPERTY_DEFINITION_REPRESENTATION(#4381,#4318);
#4277=PROPERTY_DEFINITION_REPRESENTATION(#4382,#4319);
#4278=PROPERTY_DEFINITION_REPRESENTATION(#4383,#4320);
#4279=PROPERTY_DEFINITION_REPRESENTATION(#4384,#4321);
#4280=PROPERTY_DEFINITION_REPRESENTATION(#4385,#4322);
#4281=PROPERTY_DEFINITION_REPRESENTATION(#4386,#4323);
#4282=PROPERTY_DEFINITION_REPRESENTATION(#4387,#4324);
#4283=PROPERTY_DEFINITION_REPRESENTATION(#4388,#4325);
#4284=PROPERTY_DEFINITION_REPRESENTATION(#4389,#4326);
#4285=PROPERTY_DEFINITION_REPRESENTATION(#4390,#4327);
#4286=PROPERTY_DEFINITION_REPRESENTATION(#4391,#4328);
#4287=PROPERTY_DEFINITION_REPRESENTATION(#4392,#4329);
#4288=PROPERTY_DEFINITION_REPRESENTATION(#4393,#4330);
#4289=PROPERTY_DEFINITION_REPRESENTATION(#4394,#4331);
#4290=PROPERTY_DEFINITION_REPRESENTATION(#4395,#4332);
#4291=PROPERTY_DEFINITION_REPRESENTATION(#4396,#4333);
#4292=PROPERTY_DEFINITION_REPRESENTATION(#4397,#4334);
#4293=PROPERTY_DEFINITION_REPRESENTATION(#4398,#4335);
#4294=PROPERTY_DEFINITION_REPRESENTATION(#4399,#4336);
#4295=PROPERTY_DEFINITION_REPRESENTATION(#4400,#4337);
#4296=PROPERTY_DEFINITION_REPRESENTATION(#4401,#4338);
#4297=PROPERTY_DEFINITION_REPRESENTATION(#4402,#4339);
#4298=PROPERTY_DEFINITION_REPRESENTATION(#4403,#4340);
#4299=REPRESENTATION('material name',(#4341),#7321);
#4300=REPRESENTATION('density',(#4236),#7321);
#4301=REPRESENTATION('material name',(#4342),#7322);
#4302=REPRESENTATION('density',(#4237),#7322);
#4303=REPRESENTATION('material name',(#4343),#7323);
#4304=REPRESENTATION('density',(#4238),#7323);
#4305=REPRESENTATION('material name',(#4344),#7324);
#4306=REPRESENTATION('density',(#4239),#7324);
#4307=REPRESENTATION('material name',(#4345),#7325);
#4308=REPRESENTATION('density',(#4240),#7325);
#4309=REPRESENTATION('material name',(#4346),#7326);
#4310=REPRESENTATION('density',(#4241),#7326);
#4311=REPRESENTATION('material name',(#4347),#7327);
#4312=REPRESENTATION('density',(#4242),#7327);
#4313=REPRESENTATION('material name',(#4348),#7328);
#4314=REPRESENTATION('density',(#4243),#7328);
#4315=REPRESENTATION('material name',(#4349),#7329);
#4316=REPRESENTATION('density',(#4244),#7329);
#4317=REPRESENTATION('material name',(#4350),#7330);
#4318=REPRESENTATION('density',(#4245),#7330);
#4319=REPRESENTATION('material name',(#4351),#7331);
#4320=REPRESENTATION('density',(#4246),#7331);
#4321=REPRESENTATION('material name',(#4352),#7332);
#4322=REPRESENTATION('density',(#4247),#7332);
#4323=REPRESENTATION('material name',(#4353),#7333);
#4324=REPRESENTATION('density',(#4248),#7333);
#4325=REPRESENTATION('material name',(#4354),#7335);
#4326=REPRESENTATION('density',(#4249),#7335);
#4327=REPRESENTATION('material name',(#4355),#7336);
#4328=REPRESENTATION('density',(#4250),#7336);
#4329=REPRESENTATION('material name',(#4356),#7337);
#4330=REPRESENTATION('density',(#4251),#7337);
#4331=REPRESENTATION('material name',(#4357),#7338);
#4332=REPRESENTATION('density',(#4252),#7338);
#4333=REPRESENTATION('material name',(#4358),#7339);
#4334=REPRESENTATION('density',(#4253),#7339);
#4335=REPRESENTATION('material name',(#4359),#7340);
#4336=REPRESENTATION('density',(#4254),#7340);
#4337=REPRESENTATION('material name',(#4360),#7341);
#4338=REPRESENTATION('density',(#4255),#7341);
#4339=REPRESENTATION('material name',(#4361),#7343);
#4340=REPRESENTATION('density',(#4256),#7343);
#4341=DESCRIPTIVE_REPRESENTATION_ITEM('Steel','Steel');
#4342=DESCRIPTIVE_REPRESENTATION_ITEM('Steel','Steel');
#4343=DESCRIPTIVE_REPRESENTATION_ITEM('Steel','Steel');
#4344=DESCRIPTIVE_REPRESENTATION_ITEM('Steel','Steel');
#4345=DESCRIPTIVE_REPRESENTATION_ITEM('Steel','Steel');
#4346=DESCRIPTIVE_REPRESENTATION_ITEM('Steel','Steel');
#4347=DESCRIPTIVE_REPRESENTATION_ITEM('Steel','Steel');
#4348=DESCRIPTIVE_REPRESENTATION_ITEM('Steel','Steel');
#4349=DESCRIPTIVE_REPRESENTATION_ITEM('Steel','Steel');
#4350=DESCRIPTIVE_REPRESENTATION_ITEM('Steel','Steel');
#4351=DESCRIPTIVE_REPRESENTATION_ITEM('Steel','Steel');
#4352=DESCRIPTIVE_REPRESENTATION_ITEM('Steel','Steel');
#4353=DESCRIPTIVE_REPRESENTATION_ITEM('Steel','Steel');
#4354=DESCRIPTIVE_REPRESENTATION_ITEM('Steel','Steel');
#4355=DESCRIPTIVE_REPRESENTATION_ITEM('Steel','Steel');
#4356=DESCRIPTIVE_REPRESENTATION_ITEM('Steel','Steel');
#4357=DESCRIPTIVE_REPRESENTATION_ITEM('Steel','Steel');
#4358=DESCRIPTIVE_REPRESENTATION_ITEM('Steel','Steel');
#4359=DESCRIPTIVE_REPRESENTATION_ITEM('Steel','Steel');
#4360=DESCRIPTIVE_REPRESENTATION_ITEM('Steel','Steel');
#4361=DESCRIPTIVE_REPRESENTATION_ITEM('Steel','Steel');
#4362=PROPERTY_DEFINITION('material property','material name',#7468);
#4363=PROPERTY_DEFINITION('material property','density of part',#7468);
#4364=PROPERTY_DEFINITION('material property','material name',#7469);
#4365=PROPERTY_DEFINITION('material property','density of part',#7469);
#4366=PROPERTY_DEFINITION('material property','material name',#7470);
#4367=PROPERTY_DEFINITION('material property','density of part',#7470);
#4368=PROPERTY_DEFINITION('material property','material name',#7471);
#4369=PROPERTY_DEFINITION('material property','density of part',#7471);
#4370=PROPERTY_DEFINITION('material property','material name',#7472);
#4371=PROPERTY_DEFINITION('material property','density of part',#7472);
#4372=PROPERTY_DEFINITION('material property','material name',#7473);
#4373=PROPERTY_DEFINITION('material property','density of part',#7473);
#4374=PROPERTY_DEFINITION('material property','material name',#7474);
#4375=PROPERTY_DEFINITION('material property','density of part',#7474);
#4376=PROPERTY_DEFINITION('material property','material name',#7475);
#4377=PROPERTY_DEFINITION('material property','density of part',#7475);
#4378=PROPERTY_DEFINITION('material property','material name',#7476);
#4379=PROPERTY_DEFINITION('material property','density of part',#7476);
#4380=PROPERTY_DEFINITION('material property','material name',#7477);
#4381=PROPERTY_DEFINITION('material property','density of part',#7477);
#4382=PROPERTY_DEFINITION('material property','material name',#7478);
#4383=PROPERTY_DEFINITION('material property','density of part',#7478);
#4384=PROPERTY_DEFINITION('material property','material name',#7479);
#4385=PROPERTY_DEFINITION('material property','density of part',#7479);
#4386=PROPERTY_DEFINITION('material property','material name',#7480);
#4387=PROPERTY_DEFINITION('material property','density of part',#7480);
#4388=PROPERTY_DEFINITION('material property','material name',#7482);
#4389=PROPERTY_DEFINITION('material property','density of part',#7482);
#4390=PROPERTY_DEFINITION('material property','material name',#7483);
#4391=PROPERTY_DEFINITION('material property','density of part',#7483);
#4392=PROPERTY_DEFINITION('material property','material name',#7484);
#4393=PROPERTY_DEFINITION('material property','density of part',#7484);
#4394=PROPERTY_DEFINITION('material property','material name',#7485);
#4395=PROPERTY_DEFINITION('material property','density of part',#7485);
#4396=PROPERTY_DEFINITION('material property','material name',#7486);
#4397=PROPERTY_DEFINITION('material property','density of part',#7486);
#4398=PROPERTY_DEFINITION('material property','material name',#7487);
#4399=PROPERTY_DEFINITION('material property','density of part',#7487);
#4400=PROPERTY_DEFINITION('material property','material name',#7488);
#4401=PROPERTY_DEFINITION('material property','density of part',#7488);
#4402=PROPERTY_DEFINITION('material property','material name',#7490);
#4403=PROPERTY_DEFINITION('material property','density of part',#7490);
#4404=AXIS2_PLACEMENT_3D('',#6086,#4843,#4844);
#4405=AXIS2_PLACEMENT_3D('',#6087,#4845,#4846);
#4406=AXIS2_PLACEMENT_3D('',#6088,#4847,#4848);
#4407=AXIS2_PLACEMENT_3D('',#6089,#4849,#4850);
#4408=AXIS2_PLACEMENT_3D('',#6098,#4855,#4856);
#4409=AXIS2_PLACEMENT_3D('',#6104,#4860,#4861);
#4410=AXIS2_PLACEMENT_3D('',#6110,#4865,#4866);
#4411=AXIS2_PLACEMENT_3D('',#6113,#4869,#4870);
#4412=AXIS2_PLACEMENT_3D('',#6114,#4871,#4872);
#4413=AXIS2_PLACEMENT_3D('',#6123,#4877,#4878);
#4414=AXIS2_PLACEMENT_3D('',#6129,#4882,#4883);
#4415=AXIS2_PLACEMENT_3D('',#6135,#4887,#4888);
#4416=AXIS2_PLACEMENT_3D('',#6138,#4891,#4892);
#4417=AXIS2_PLACEMENT_3D('',#6139,#4893,#4894);
#4418=AXIS2_PLACEMENT_3D('',#6141,#4895,#4896);
#4419=AXIS2_PLACEMENT_3D('',#6144,#4898,#4899);
#4420=AXIS2_PLACEMENT_3D('',#6145,#4900,#4901);
#4421=AXIS2_PLACEMENT_3D('',#6147,#4902,#4903);
#4422=AXIS2_PLACEMENT_3D('',#6150,#4905,#4906);
#4423=AXIS2_PLACEMENT_3D('',#6151,#4907,#4908);
#4424=AXIS2_PLACEMENT_3D('',#6153,#4909,#4910);
#4425=AXIS2_PLACEMENT_3D('',#6156,#4912,#4913);
#4426=AXIS2_PLACEMENT_3D('',#6157,#4914,#4915);
#4427=AXIS2_PLACEMENT_3D('',#6159,#4916,#4917);
#4428=AXIS2_PLACEMENT_3D('',#6162,#4919,#4920);
#4429=AXIS2_PLACEMENT_3D('',#6163,#4921,#4922);
#4430=AXIS2_PLACEMENT_3D('',#6165,#4923,#4924);
#4431=AXIS2_PLACEMENT_3D('',#6168,#4926,#4927);
#4432=AXIS2_PLACEMENT_3D('',#6169,#4928,#4929);
#4433=AXIS2_PLACEMENT_3D('',#6171,#4930,#4931);
#4434=AXIS2_PLACEMENT_3D('',#6174,#4933,#4934);
#4435=AXIS2_PLACEMENT_3D('',#6175,#4935,#4936);
#4436=AXIS2_PLACEMENT_3D('',#6177,#4937,#4938);
#4437=AXIS2_PLACEMENT_3D('',#6180,#4940,#4941);
#4438=AXIS2_PLACEMENT_3D('',#6181,#4942,#4943);
#4439=AXIS2_PLACEMENT_3D('',#6183,#4944,#4945);
#4440=AXIS2_PLACEMENT_3D('',#6186,#4947,#4948);
#4441=AXIS2_PLACEMENT_3D('',#6187,#4949,#4950);
#4442=AXIS2_PLACEMENT_3D('',#6189,#4951,#4952);
#4443=AXIS2_PLACEMENT_3D('',#6192,#4954,#4955);
#4444=AXIS2_PLACEMENT_3D('',#6193,#4956,#4957);
#4445=AXIS2_PLACEMENT_3D('',#6195,#4958,#4959);
#4446=AXIS2_PLACEMENT_3D('',#6198,#4961,#4962);
#4447=AXIS2_PLACEMENT_3D('',#6199,#4963,#4964);
#4448=AXIS2_PLACEMENT_3D('',#6201,#4965,#4966);
#4449=AXIS2_PLACEMENT_3D('',#6204,#4968,#4969);
#4450=AXIS2_PLACEMENT_3D('',#6205,#4970,#4971);
#4451=AXIS2_PLACEMENT_3D('',#6207,#4972,#4973);
#4452=AXIS2_PLACEMENT_3D('',#6210,#4975,#4976);
#4453=AXIS2_PLACEMENT_3D('',#6211,#4977,#4978);
#4454=AXIS2_PLACEMENT_3D('',#6220,#4983,#4984);
#4455=AXIS2_PLACEMENT_3D('',#6226,#4988,#4989);
#4456=AXIS2_PLACEMENT_3D('',#6232,#4993,#4994);
#4457=AXIS2_PLACEMENT_3D('',#6235,#4997,#4998);
#4458=AXIS2_PLACEMENT_3D('',#6236,#4999,#5000);
#4459=AXIS2_PLACEMENT_3D('',#6237,#5001,#5002);
#4460=AXIS2_PLACEMENT_3D('',#6238,#5003,#5004);
#4461=AXIS2_PLACEMENT_3D('',#6240,#5005,#5006);
#4462=AXIS2_PLACEMENT_3D('',#6243,#5008,#5009);
#4463=AXIS2_PLACEMENT_3D('',#6244,#5010,#5011);
#4464=AXIS2_PLACEMENT_3D('',#6246,#5012,#5013);
#4465=AXIS2_PLACEMENT_3D('',#6249,#5015,#5016);
#4466=AXIS2_PLACEMENT_3D('',#6250,#5017,#5018);
#4467=AXIS2_PLACEMENT_3D('',#6259,#5023,#5024);
#4468=AXIS2_PLACEMENT_3D('',#6265,#5028,#5029);
#4469=AXIS2_PLACEMENT_3D('',#6271,#5033,#5034);
#4470=AXIS2_PLACEMENT_3D('',#6274,#5037,#5038);
#4471=AXIS2_PLACEMENT_3D('',#6275,#5039,#5040);
#4472=AXIS2_PLACEMENT_3D('',#6276,#5041,#5042);
#4473=AXIS2_PLACEMENT_3D('',#6277,#5043,#5044);
#4474=AXIS2_PLACEMENT_3D('',#6286,#5049,#5050);
#4475=AXIS2_PLACEMENT_3D('',#6292,#5054,#5055);
#4476=AXIS2_PLACEMENT_3D('',#6298,#5059,#5060);
#4477=AXIS2_PLACEMENT_3D('',#6301,#5063,#5064);
#4478=AXIS2_PLACEMENT_3D('',#6302,#5065,#5066);
#4479=AXIS2_PLACEMENT_3D('',#6303,#5067,#5068);
#4480=AXIS2_PLACEMENT_3D('',#6304,#5069,#5070);
#4481=AXIS2_PLACEMENT_3D('',#6306,#5071,#5072);
#4482=AXIS2_PLACEMENT_3D('',#6309,#5074,#5075);
#4483=AXIS2_PLACEMENT_3D('',#6310,#5076,#5077);
#4484=AXIS2_PLACEMENT_3D('',#6312,#5078,#5079);
#4485=AXIS2_PLACEMENT_3D('',#6315,#5081,#5082);
#4486=AXIS2_PLACEMENT_3D('',#6316,#5083,#5084);
#4487=AXIS2_PLACEMENT_3D('',#6325,#5089,#5090);
#4488=AXIS2_PLACEMENT_3D('',#6331,#5094,#5095);
#4489=AXIS2_PLACEMENT_3D('',#6337,#5099,#5100);
#4490=AXIS2_PLACEMENT_3D('',#6340,#5103,#5104);
#4491=AXIS2_PLACEMENT_3D('',#6341,#5105,#5106);
#4492=AXIS2_PLACEMENT_3D('',#6342,#5107,#5108);
#4493=AXIS2_PLACEMENT_3D('',#6343,#5109,#5110);
#4494=AXIS2_PLACEMENT_3D('',#6352,#5115,#5116);
#4495=AXIS2_PLACEMENT_3D('',#6358,#5120,#5121);
#4496=AXIS2_PLACEMENT_3D('',#6364,#5125,#5126);
#4497=AXIS2_PLACEMENT_3D('',#6367,#5129,#5130);
#4498=AXIS2_PLACEMENT_3D('',#6368,#5131,#5132);
#4499=AXIS2_PLACEMENT_3D('',#6369,#5133,#5134);
#4500=AXIS2_PLACEMENT_3D('',#6370,#5135,#5136);
#4501=AXIS2_PLACEMENT_3D('',#6375,#5138,#5139);
#4502=AXIS2_PLACEMENT_3D('',#6378,#5141,#5142);
#4503=AXIS2_PLACEMENT_3D('',#6379,#5143,#5144);
#4504=AXIS2_PLACEMENT_3D('',#6384,#5146,#5147);
#4505=AXIS2_PLACEMENT_3D('',#6388,#5149,#5150);
#4506=AXIS2_PLACEMENT_3D('',#6389,#5151,#5152);
#4507=AXIS2_PLACEMENT_3D('',#6390,#5153,#5154);
#4508=AXIS2_PLACEMENT_3D('',#6399,#5159,#5160);
#4509=AXIS2_PLACEMENT_3D('',#6405,#5164,#5165);
#4510=AXIS2_PLACEMENT_3D('',#6411,#5169,#5170);
#4511=AXIS2_PLACEMENT_3D('',#6414,#5173,#5174);
#4512=AXIS2_PLACEMENT_3D('',#6415,#5175,#5176);
#4513=AXIS2_PLACEMENT_3D('',#6416,#5177,#5178);
#4514=AXIS2_PLACEMENT_3D('',#6418,#5180,#5181);
#4515=AXIS2_PLACEMENT_3D('',#6419,#5182,#5183);
#4516=AXIS2_PLACEMENT_3D('',#6421,#5184,#5185);
#4517=AXIS2_PLACEMENT_3D('',#6422,#5186,#5187);
#4518=AXIS2_PLACEMENT_3D('',#6424,#5188,#5189);
#4519=AXIS2_PLACEMENT_3D('',#6425,#5190,#5191);
#4520=AXIS2_PLACEMENT_3D('',#6427,#5193,#5194);
#4521=AXIS2_PLACEMENT_3D('',#6428,#5195,#5196);
#4522=AXIS2_PLACEMENT_3D('',#6430,#5197,#5198);
#4523=AXIS2_PLACEMENT_3D('',#6431,#5199,#5200);
#4524=AXIS2_PLACEMENT_3D('',#6441,#5206,#5207);
#4525=AXIS2_PLACEMENT_3D('',#6445,#5210,#5211);
#4526=AXIS2_PLACEMENT_3D('',#6452,#5216,#5217);
#4527=AXIS2_PLACEMENT_3D('',#6456,#5220,#5221);
#4528=AXIS2_PLACEMENT_3D('',#6458,#5222,#5223);
#4529=AXIS2_PLACEMENT_3D('',#6460,#5225,#5226);
#4530=AXIS2_PLACEMENT_3D('',#6462,#5227,#5228);
#4531=AXIS2_PLACEMENT_3D('',#6464,#5230,#5231);
#4532=AXIS2_PLACEMENT_3D('',#6468,#5234,#5235);
#4533=AXIS2_PLACEMENT_3D('',#6472,#5238,#5239);
#4534=AXIS2_PLACEMENT_3D('',#6478,#5243,#5244);
#4535=AXIS2_PLACEMENT_3D('',#6482,#5247,#5248);
#4536=AXIS2_PLACEMENT_3D('',#6486,#5251,#5252);
#4537=AXIS2_PLACEMENT_3D('',#6488,#5254,#5255);
#4538=AXIS2_PLACEMENT_3D('',#6489,#5256,#5257);
#4539=AXIS2_PLACEMENT_3D('',#6490,#5258,#5259);
#4540=AXIS2_PLACEMENT_3D('',#6495,#5261,#5262);
#4541=AXIS2_PLACEMENT_3D('',#6498,#5264,#5265);
#4542=AXIS2_PLACEMENT_3D('',#6499,#5266,#5267);
#4543=AXIS2_PLACEMENT_3D('',#6504,#5269,#5270);
#4544=AXIS2_PLACEMENT_3D('',#6508,#5272,#5273);
#4545=AXIS2_PLACEMENT_3D('',#6509,#5274,#5275);
#4546=AXIS2_PLACEMENT_3D('',#6510,#5276,#5277);
#4547=AXIS2_PLACEMENT_3D('',#6519,#5282,#5283);
#4548=AXIS2_PLACEMENT_3D('',#6525,#5287,#5288);
#4549=AXIS2_PLACEMENT_3D('',#6531,#5292,#5293);
#4550=AXIS2_PLACEMENT_3D('',#6534,#5296,#5297);
#4551=AXIS2_PLACEMENT_3D('',#6535,#5298,#5299);
#4552=AXIS2_PLACEMENT_3D('',#6536,#5300,#5301);
#4553=AXIS2_PLACEMENT_3D('',#6538,#5303,#5304);
#4554=AXIS2_PLACEMENT_3D('',#6539,#5305,#5306);
#4555=AXIS2_PLACEMENT_3D('',#6541,#5307,#5308);
#4556=AXIS2_PLACEMENT_3D('',#6542,#5309,#5310);
#4557=AXIS2_PLACEMENT_3D('',#6544,#5311,#5312);
#4558=AXIS2_PLACEMENT_3D('',#6545,#5313,#5314);
#4559=AXIS2_PLACEMENT_3D('',#6547,#5316,#5317);
#4560=AXIS2_PLACEMENT_3D('',#6548,#5318,#5319);
#4561=AXIS2_PLACEMENT_3D('',#6550,#5320,#5321);
#4562=AXIS2_PLACEMENT_3D('',#6551,#5322,#5323);
#4563=AXIS2_PLACEMENT_3D('',#6561,#5329,#5330);
#4564=AXIS2_PLACEMENT_3D('',#6565,#5333,#5334);
#4565=AXIS2_PLACEMENT_3D('',#6572,#5339,#5340);
#4566=AXIS2_PLACEMENT_3D('',#6576,#5343,#5344);
#4567=AXIS2_PLACEMENT_3D('',#6578,#5345,#5346);
#4568=AXIS2_PLACEMENT_3D('',#6580,#5348,#5349);
#4569=AXIS2_PLACEMENT_3D('',#6582,#5350,#5351);
#4570=AXIS2_PLACEMENT_3D('',#6584,#5353,#5354);
#4571=AXIS2_PLACEMENT_3D('',#6588,#5357,#5358);
#4572=AXIS2_PLACEMENT_3D('',#6592,#5361,#5362);
#4573=AXIS2_PLACEMENT_3D('',#6598,#5366,#5367);
#4574=AXIS2_PLACEMENT_3D('',#6602,#5370,#5371);
#4575=AXIS2_PLACEMENT_3D('',#6606,#5374,#5375);
#4576=AXIS2_PLACEMENT_3D('',#6608,#5377,#5378);
#4577=AXIS2_PLACEMENT_3D('',#6609,#5379,#5380);
#4578=AXIS2_PLACEMENT_3D('',#6610,#5381,#5382);
#4579=AXIS2_PLACEMENT_3D('',#6612,#5383,#5384);
#4580=AXIS2_PLACEMENT_3D('',#6615,#5386,#5387);
#4581=AXIS2_PLACEMENT_3D('',#6616,#5388,#5389);
#4582=AXIS2_PLACEMENT_3D('',#6621,#5391,#5392);
#4583=AXIS2_PLACEMENT_3D('',#6624,#5394,#5395);
#4584=AXIS2_PLACEMENT_3D('',#6625,#5396,#5397);
#4585=AXIS2_PLACEMENT_3D('',#6627,#5399,#5400);
#4586=AXIS2_PLACEMENT_3D('',#6629,#5402,#5403);
#4587=AXIS2_PLACEMENT_3D('',#6630,#5404,#5405);
#4588=AXIS2_PLACEMENT_3D('',#6632,#5406,#5407);
#4589=AXIS2_PLACEMENT_3D('',#6633,#5408,#5409);
#4590=AXIS2_PLACEMENT_3D('',#6638,#5411,#5412);
#4591=AXIS2_PLACEMENT_3D('',#6641,#5414,#5415);
#4592=AXIS2_PLACEMENT_3D('',#6642,#5416,#5417);
#4593=AXIS2_PLACEMENT_3D('',#6644,#5419,#5420);
#4594=AXIS2_PLACEMENT_3D('',#6646,#5422,#5423);
#4595=AXIS2_PLACEMENT_3D('',#6647,#5424,#5425);
#4596=AXIS2_PLACEMENT_3D('',#6649,#5426,#5427);
#4597=AXIS2_PLACEMENT_3D('',#6650,#5428,#5429);
#4598=AXIS2_PLACEMENT_3D('',#6656,#5433,#5434);
#4599=AXIS2_PLACEMENT_3D('',#6659,#5437,#5438);
#4600=AXIS2_PLACEMENT_3D('',#6665,#5442,#5443);
#4601=AXIS2_PLACEMENT_3D('',#6667,#5444,#5445);
#4602=AXIS2_PLACEMENT_3D('',#6669,#5447,#5448);
#4603=AXIS2_PLACEMENT_3D('',#6671,#5449,#5450);
#4604=AXIS2_PLACEMENT_3D('',#6673,#5452,#5453);
#4605=AXIS2_PLACEMENT_3D('',#6679,#5457,#5458);
#4606=AXIS2_PLACEMENT_3D('',#6683,#5461,#5462);
#4607=AXIS2_PLACEMENT_3D('',#6687,#5465,#5466);
#4608=AXIS2_PLACEMENT_3D('',#6689,#5468,#5469);
#4609=AXIS2_PLACEMENT_3D('',#6690,#5470,#5471);
#4610=AXIS2_PLACEMENT_3D('',#6691,#5472,#5473);
#4611=AXIS2_PLACEMENT_3D('',#6708,#5482,#5483);
#4612=AXIS2_PLACEMENT_3D('',#6714,#5487,#5488);
#4613=AXIS2_PLACEMENT_3D('',#6718,#5491,#5492);
#4614=AXIS2_PLACEMENT_3D('',#6722,#5495,#5496);
#4615=AXIS2_PLACEMENT_3D('',#6726,#5499,#5500);
#4616=AXIS2_PLACEMENT_3D('',#6734,#5505,#5506);
#4617=AXIS2_PLACEMENT_3D('',#6736,#5508,#5509);
#4618=AXIS2_PLACEMENT_3D('',#6738,#5511,#5512);
#4619=AXIS2_PLACEMENT_3D('',#6740,#5514,#5515);
#4620=AXIS2_PLACEMENT_3D('',#6741,#5516,#5517);
#4621=AXIS2_PLACEMENT_3D('',#6742,#5518,#5519);
#4622=AXIS2_PLACEMENT_3D('',#6744,#5520,#5521);
#4623=AXIS2_PLACEMENT_3D('',#6745,#5522,#5523);
#4624=AXIS2_PLACEMENT_3D('',#6747,#5524,#5525);
#4625=AXIS2_PLACEMENT_3D('',#6749,#5527,#5528);
#4626=AXIS2_PLACEMENT_3D('',#6751,#5529,#5530);
#4627=AXIS2_PLACEMENT_3D('',#6753,#5532,#5533);
#4628=AXIS2_PLACEMENT_3D('',#6755,#5534,#5535);
#4629=AXIS2_PLACEMENT_3D('',#6757,#5537,#5538);
#4630=AXIS2_PLACEMENT_3D('',#6759,#5539,#5540);
#4631=AXIS2_PLACEMENT_3D('',#6760,#5541,#5542);
#4632=AXIS2_PLACEMENT_3D('',#6762,#5543,#5544);
#4633=AXIS2_PLACEMENT_3D('',#6764,#5546,#5547);
#4634=AXIS2_PLACEMENT_3D('',#6766,#5548,#5549);
#4635=AXIS2_PLACEMENT_3D('',#6768,#5551,#5552);
#4636=AXIS2_PLACEMENT_3D('',#6770,#5553,#5554);
#4637=AXIS2_PLACEMENT_3D('',#6772,#5556,#5557);
#4638=AXIS2_PLACEMENT_3D('',#6773,#5558,#5559);
#4639=AXIS2_PLACEMENT_3D('',#6782,#5564,#5565);
#4640=AXIS2_PLACEMENT_3D('',#6788,#5569,#5570);
#4641=AXIS2_PLACEMENT_3D('',#6794,#5574,#5575);
#4642=AXIS2_PLACEMENT_3D('',#6800,#5579,#5580);
#4643=AXIS2_PLACEMENT_3D('',#6806,#5584,#5585);
#4644=AXIS2_PLACEMENT_3D('',#6809,#5588,#5589);
#4645=AXIS2_PLACEMENT_3D('',#6810,#5590,#5591);
#4646=AXIS2_PLACEMENT_3D('',#6811,#5592,#5593);
#4647=AXIS2_PLACEMENT_3D('',#6812,#5594,#5595);
#4648=AXIS2_PLACEMENT_3D('',#6814,#5596,#5597);
#4649=AXIS2_PLACEMENT_3D('',#6815,#5598,#5599);
#4650=AXIS2_PLACEMENT_3D('',#6817,#5600,#5601);
#4651=AXIS2_PLACEMENT_3D('',#6819,#5603,#5604);
#4652=AXIS2_PLACEMENT_3D('',#6821,#5605,#5606);
#4653=AXIS2_PLACEMENT_3D('',#6823,#5608,#5609);
#4654=AXIS2_PLACEMENT_3D('',#6825,#5610,#5611);
#4655=AXIS2_PLACEMENT_3D('',#6827,#5613,#5614);
#4656=AXIS2_PLACEMENT_3D('',#6829,#5615,#5616);
#4657=AXIS2_PLACEMENT_3D('',#6830,#5617,#5618);
#4658=AXIS2_PLACEMENT_3D('',#6832,#5619,#5620);
#4659=AXIS2_PLACEMENT_3D('',#6834,#5622,#5623);
#4660=AXIS2_PLACEMENT_3D('',#6836,#5624,#5625);
#4661=AXIS2_PLACEMENT_3D('',#6838,#5627,#5628);
#4662=AXIS2_PLACEMENT_3D('',#6840,#5629,#5630);
#4663=AXIS2_PLACEMENT_3D('',#6842,#5632,#5633);
#4664=AXIS2_PLACEMENT_3D('',#6843,#5634,#5635);
#4665=AXIS2_PLACEMENT_3D('',#6852,#5640,#5641);
#4666=AXIS2_PLACEMENT_3D('',#6858,#5645,#5646);
#4667=AXIS2_PLACEMENT_3D('',#6864,#5650,#5651);
#4668=AXIS2_PLACEMENT_3D('',#6870,#5655,#5656);
#4669=AXIS2_PLACEMENT_3D('',#6876,#5660,#5661);
#4670=AXIS2_PLACEMENT_3D('',#6879,#5664,#5665);
#4671=AXIS2_PLACEMENT_3D('',#6880,#5666,#5667);
#4672=AXIS2_PLACEMENT_3D('',#6881,#5668,#5669);
#4673=AXIS2_PLACEMENT_3D('',#6882,#5670,#5671);
#4674=AXIS2_PLACEMENT_3D('',#6884,#5672,#5673);
#4675=AXIS2_PLACEMENT_3D('',#6887,#5675,#5676);
#4676=AXIS2_PLACEMENT_3D('',#6888,#5677,#5678);
#4677=AXIS2_PLACEMENT_3D('',#6890,#5679,#5680);
#4678=AXIS2_PLACEMENT_3D('',#6893,#5682,#5683);
#4679=AXIS2_PLACEMENT_3D('',#6894,#5684,#5685);
#4680=AXIS2_PLACEMENT_3D('',#6895,#5686,#5687);
#4681=AXIS2_PLACEMENT_3D('',#6896,#5688,#5689);
#4682=AXIS2_PLACEMENT_3D('',#6897,#5690,#5691);
#4683=AXIS2_PLACEMENT_3D('',#6909,#5693,#5694);
#4684=AXIS2_PLACEMENT_3D('',#6925,#5695,#5696);
#4685=AXIS2_PLACEMENT_3D('',#6927,#5697,#5698);
#4686=AXIS2_PLACEMENT_3D('',#6953,#5700,#5701);
#4687=AXIS2_PLACEMENT_3D('',#6956,#5704,#5705);
#4688=AXIS2_PLACEMENT_3D('',#6958,#5707,#5708);
#4689=AXIS2_PLACEMENT_3D('',#6960,#5710,#5711);
#4690=AXIS2_PLACEMENT_3D('',#6962,#5712,#5713);
#4691=AXIS2_PLACEMENT_3D('',#6965,#5715,#5716);
#4692=AXIS2_PLACEMENT_3D('',#6966,#5717,#5718);
#4693=AXIS2_PLACEMENT_3D('',#6968,#5720,#5721);
#4694=AXIS2_PLACEMENT_3D('',#6970,#5723,#5724);
#4695=AXIS2_PLACEMENT_3D('',#6971,#5725,#5726);
#4696=AXIS2_PLACEMENT_3D('',#6972,#5727,#5728);
#4697=AXIS2_PLACEMENT_3D('',#6973,#5729,#5730);
#4698=AXIS2_PLACEMENT_3D('',#6974,#5731,#5732);
#4699=AXIS2_PLACEMENT_3D('',#6975,#5733,#5734);
#4700=AXIS2_PLACEMENT_3D('',#6976,#5735,#5736);
#4701=AXIS2_PLACEMENT_3D('',#6977,#5737,#5738);
#4702=AXIS2_PLACEMENT_3D('',#6978,#5739,#5740);
#4703=AXIS2_PLACEMENT_3D('',#6979,#5741,#5742);
#4704=AXIS2_PLACEMENT_3D('',#6980,#5743,#5744);
#4705=AXIS2_PLACEMENT_3D('',#6981,#5745,#5746);
#4706=AXIS2_PLACEMENT_3D('',#6982,#5747,#5748);
#4707=AXIS2_PLACEMENT_3D('',#6983,#5749,#5750);
#4708=AXIS2_PLACEMENT_3D('',#6984,#5751,#5752);
#4709=AXIS2_PLACEMENT_3D('',#6985,#5753,#5754);
#4710=AXIS2_PLACEMENT_3D('',#6986,#5755,#5756);
#4711=AXIS2_PLACEMENT_3D('',#6987,#5757,#5758);
#4712=AXIS2_PLACEMENT_3D('',#6988,#5759,#5760);
#4713=AXIS2_PLACEMENT_3D('',#6989,#5761,#5762);
#4714=AXIS2_PLACEMENT_3D('',#6990,#5763,#5764);
#4715=AXIS2_PLACEMENT_3D('',#6991,#5765,#5766);
#4716=AXIS2_PLACEMENT_3D('',#6992,#5767,#5768);
#4717=AXIS2_PLACEMENT_3D('',#6993,#5769,#5770);
#4718=AXIS2_PLACEMENT_3D('',#6994,#5771,#5772);
#4719=AXIS2_PLACEMENT_3D('',#6995,#5773,#5774);
#4720=AXIS2_PLACEMENT_3D('',#6996,#5775,#5776);
#4721=AXIS2_PLACEMENT_3D('',#6997,#5777,#5778);
#4722=AXIS2_PLACEMENT_3D('',#6998,#5779,#5780);
#4723=AXIS2_PLACEMENT_3D('',#7000,#5781,#5782);
#4724=AXIS2_PLACEMENT_3D('',#7003,#5784,#5785);
#4725=AXIS2_PLACEMENT_3D('',#7004,#5786,#5787);
#4726=AXIS2_PLACEMENT_3D('',#7006,#5788,#5789);
#4727=AXIS2_PLACEMENT_3D('',#7009,#5791,#5792);
#4728=AXIS2_PLACEMENT_3D('',#7010,#5793,#5794);
#4729=AXIS2_PLACEMENT_3D('',#7012,#5795,#5796);
#4730=AXIS2_PLACEMENT_3D('',#7015,#5798,#5799);
#4731=AXIS2_PLACEMENT_3D('',#7016,#5800,#5801);
#4732=AXIS2_PLACEMENT_3D('',#7018,#5802,#5803);
#4733=AXIS2_PLACEMENT_3D('',#7021,#5805,#5806);
#4734=AXIS2_PLACEMENT_3D('',#7022,#5807,#5808);
#4735=AXIS2_PLACEMENT_3D('',#7031,#5813,#5814);
#4736=AXIS2_PLACEMENT_3D('',#7037,#5818,#5819);
#4737=AXIS2_PLACEMENT_3D('',#7043,#5823,#5824);
#4738=AXIS2_PLACEMENT_3D('',#7046,#5827,#5828);
#4739=AXIS2_PLACEMENT_3D('',#7047,#5829,#5830);
#4740=AXIS2_PLACEMENT_3D('',#7048,#5831,#5832);
#4741=AXIS2_PLACEMENT_3D('',#7049,#5833,#5834);
#4742=AXIS2_PLACEMENT_3D('',#7051,#5835,#5836);
#4743=AXIS2_PLACEMENT_3D('',#7054,#5838,#5839);
#4744=AXIS2_PLACEMENT_3D('',#7055,#5840,#5841);
#4745=AXIS2_PLACEMENT_3D('',#7056,#5842,#5843);
#4746=AXIS2_PLACEMENT_3D('',#7058,#5844,#5845);
#4747=AXIS2_PLACEMENT_3D('',#7061,#5847,#5848);
#4748=AXIS2_PLACEMENT_3D('',#7062,#5849,#5850);
#4749=AXIS2_PLACEMENT_3D('',#7063,#5851,#5852);
#4750=AXIS2_PLACEMENT_3D('',#7068,#5854,#5855);
#4751=AXIS2_PLACEMENT_3D('',#7071,#5857,#5858);
#4752=AXIS2_PLACEMENT_3D('',#7072,#5859,#5860);
#4753=AXIS2_PLACEMENT_3D('',#7078,#5864,#5865);
#4754=AXIS2_PLACEMENT_3D('',#7082,#5868,#5869);
#4755=AXIS2_PLACEMENT_3D('',#7086,#5872,#5873);
#4756=AXIS2_PLACEMENT_3D('',#7088,#5875,#5876);
#4757=AXIS2_PLACEMENT_3D('',#7089,#5877,#5878);
#4758=AXIS2_PLACEMENT_3D('',#7090,#5879,#5880);
#4759=AXIS2_PLACEMENT_3D('',#7092,#5881,#5882);
#4760=AXIS2_PLACEMENT_3D('',#7095,#5884,#5885);
#4761=AXIS2_PLACEMENT_3D('',#7096,#5886,#5887);
#4762=AXIS2_PLACEMENT_3D('',#7097,#5888,#5889);
#4763=AXIS2_PLACEMENT_3D('',#7098,#5890,#5891);
#4764=AXIS2_PLACEMENT_3D('',#7099,#5892,#5893);
#4765=AXIS2_PLACEMENT_3D('',#7101,#5894,#5895);
#4766=AXIS2_PLACEMENT_3D('',#7104,#5897,#5898);
#4767=AXIS2_PLACEMENT_3D('',#7105,#5899,#5900);
#4768=AXIS2_PLACEMENT_3D('',#7106,#5901,#5902);
#4769=AXIS2_PLACEMENT_3D('',#7107,#5903,#5904);
#4770=AXIS2_PLACEMENT_3D('',#7108,#5905,#5906);
#4771=AXIS2_PLACEMENT_3D('',#7117,#5911,#5912);
#4772=AXIS2_PLACEMENT_3D('',#7123,#5916,#5917);
#4773=AXIS2_PLACEMENT_3D('',#7129,#5921,#5922);
#4774=AXIS2_PLACEMENT_3D('',#7135,#5926,#5927);
#4775=AXIS2_PLACEMENT_3D('',#7141,#5931,#5932);
#4776=AXIS2_PLACEMENT_3D('',#7144,#5935,#5936);
#4777=AXIS2_PLACEMENT_3D('',#7145,#5937,#5938);
#4778=AXIS2_PLACEMENT_3D('',#7146,#5939,#5940);
#4779=AXIS2_PLACEMENT_3D('',#7148,#5941,#5942);
#4780=AXIS2_PLACEMENT_3D('',#7149,#5943,#5944);
#4781=AXIS2_PLACEMENT_3D('',#7151,#5945,#5946);
#4782=AXIS2_PLACEMENT_3D('',#7152,#5947,#5948);
#4783=AXIS2_PLACEMENT_3D('',#7154,#5949,#5950);
#4784=AXIS2_PLACEMENT_3D('',#7156,#5952,#5953);
#4785=AXIS2_PLACEMENT_3D('',#7158,#5954,#5955);
#4786=AXIS2_PLACEMENT_3D('',#7160,#5957,#5958);
#4787=AXIS2_PLACEMENT_3D('',#7162,#5959,#5960);
#4788=AXIS2_PLACEMENT_3D('',#7164,#5962,#5963);
#4789=AXIS2_PLACEMENT_3D('',#7166,#5964,#5965);
#4790=AXIS2_PLACEMENT_3D('',#7167,#5966,#5967);
#4791=AXIS2_PLACEMENT_3D('',#7169,#5968,#5969);
#4792=AXIS2_PLACEMENT_3D('',#7171,#5971,#5972);
#4793=AXIS2_PLACEMENT_3D('',#7173,#5974,#5975);
#4794=AXIS2_PLACEMENT_3D('',#7174,#5976,#5977);
#4795=AXIS2_PLACEMENT_3D('',#7176,#5978,#5979);
#4796=AXIS2_PLACEMENT_3D('',#7179,#5981,#5982);
#4797=AXIS2_PLACEMENT_3D('',#7180,#5983,#5984);
#4798=AXIS2_PLACEMENT_3D('',#7182,#5985,#5986);
#4799=AXIS2_PLACEMENT_3D('',#7185,#5988,#5989);
#4800=AXIS2_PLACEMENT_3D('',#7186,#5990,#5991);
#4801=AXIS2_PLACEMENT_3D('',#7187,#5992,#5993);
#4802=AXIS2_PLACEMENT_3D('',#7188,#5994,#5995);
#4803=AXIS2_PLACEMENT_3D('',#7189,#5996,#5997);
#4804=AXIS2_PLACEMENT_3D('',#7201,#5999,#6000);
#4805=AXIS2_PLACEMENT_3D('',#7217,#6001,#6002);
#4806=AXIS2_PLACEMENT_3D('',#7219,#6003,#6004);
#4807=AXIS2_PLACEMENT_3D('',#7245,#6006,#6007);
#4808=AXIS2_PLACEMENT_3D('',#7248,#6010,#6011);
#4809=AXIS2_PLACEMENT_3D('',#7250,#6013,#6014);
#4810=AXIS2_PLACEMENT_3D('',#7252,#6016,#6017);
#4811=AXIS2_PLACEMENT_3D('',#7254,#6018,#6019);
#4812=AXIS2_PLACEMENT_3D('',#7257,#6021,#6022);
#4813=AXIS2_PLACEMENT_3D('',#7258,#6023,#6024);
#4814=AXIS2_PLACEMENT_3D('',#7260,#6026,#6027);
#4815=AXIS2_PLACEMENT_3D('',#7262,#6029,#6030);
#4816=AXIS2_PLACEMENT_3D('',#7263,#6031,#6032);
#4817=AXIS2_PLACEMENT_3D('',#7264,#6033,#6034);
#4818=AXIS2_PLACEMENT_3D('',#7265,#6035,#6036);
#4819=AXIS2_PLACEMENT_3D('',#7266,#6037,#6038);
#4820=AXIS2_PLACEMENT_3D('',#7267,#6039,#6040);
#4821=AXIS2_PLACEMENT_3D('',#7268,#6041,#6042);
#4822=AXIS2_PLACEMENT_3D('',#7269,#6043,#6044);
#4823=AXIS2_PLACEMENT_3D('',#7270,#6045,#6046);
#4824=AXIS2_PLACEMENT_3D('',#7271,#6047,#6048);
#4825=AXIS2_PLACEMENT_3D('',#7272,#6049,#6050);
#4826=AXIS2_PLACEMENT_3D('',#7273,#6051,#6052);
#4827=AXIS2_PLACEMENT_3D('',#7274,#6053,#6054);
#4828=AXIS2_PLACEMENT_3D('',#7275,#6055,#6056);
#4829=AXIS2_PLACEMENT_3D('',#7276,#6057,#6058);
#4830=AXIS2_PLACEMENT_3D('',#7277,#6059,#6060);
#4831=AXIS2_PLACEMENT_3D('',#7278,#6061,#6062);
#4832=AXIS2_PLACEMENT_3D('',#7279,#6063,#6064);
#4833=AXIS2_PLACEMENT_3D('',#7280,#6065,#6066);
#4834=AXIS2_PLACEMENT_3D('',#7281,#6067,#6068);
#4835=AXIS2_PLACEMENT_3D('',#7283,#6069,#6070);
#4836=AXIS2_PLACEMENT_3D('',#7286,#6072,#6073);
#4837=AXIS2_PLACEMENT_3D('',#7287,#6074,#6075);
#4838=AXIS2_PLACEMENT_3D('',#7288,#6076,#6077);
#4839=AXIS2_PLACEMENT_3D('',#7289,#6078,#6079);
#4840=AXIS2_PLACEMENT_3D('',#7290,#6080,#6081);
#4841=AXIS2_PLACEMENT_3D('',#7291,#6082,#6083);
#4842=AXIS2_PLACEMENT_3D('',#7292,#6084,#6085);
#4843=DIRECTION('axis',(0.,0.,1.));
#4844=DIRECTION('refdir',(1.,0.,0.));
#4845=DIRECTION('axis',(0.,0.,1.));
#4846=DIRECTION('refdir',(1.,0.,0.));
#4847=DIRECTION('axis',(0.,0.,1.));
#4848=DIRECTION('refdir',(1.,0.,0.));
#4849=DIRECTION('center_axis',(0.,-1.,0.));
#4850=DIRECTION('ref_axis',(1.,0.,0.));
#4851=DIRECTION('',(-1.,0.,0.));
#4852=DIRECTION('',(0.,0.,1.));
#4853=DIRECTION('',(1.,0.,0.));
#4854=DIRECTION('',(0.,0.,1.));
#4855=DIRECTION('center_axis',(-1.,0.,0.));
#4856=DIRECTION('ref_axis',(0.,-1.,0.));
#4857=DIRECTION('',(0.,1.,0.));
#4858=DIRECTION('',(0.,-1.,0.));
#4859=DIRECTION('',(0.,0.,1.));
#4860=DIRECTION('center_axis',(0.,1.,0.));
#4861=DIRECTION('ref_axis',(-1.,0.,0.));
#4862=DIRECTION('',(1.,0.,0.));
#4863=DIRECTION('',(-1.,0.,0.));
#4864=DIRECTION('',(0.,0.,1.));
#4865=DIRECTION('center_axis',(1.,0.,0.));
#4866=DIRECTION('ref_axis',(0.,1.,0.));
#4867=DIRECTION('',(0.,-1.,0.));
#4868=DIRECTION('',(0.,1.,0.));
#4869=DIRECTION('center_axis',(0.,0.,1.));
#4870=DIRECTION('ref_axis',(1.,0.,0.));
#4871=DIRECTION('center_axis',(0.,-1.,0.));
#4872=DIRECTION('ref_axis',(1.,0.,0.));
#4873=DIRECTION('',(-1.,0.,0.));
#4874=DIRECTION('',(0.,0.,1.));
#4875=DIRECTION('',(1.,0.,0.));
#4876=DIRECTION('',(0.,0.,1.));
#4877=DIRECTION('center_axis',(-1.,0.,0.));
#4878=DIRECTION('ref_axis',(0.,-1.,0.));
#4879=DIRECTION('',(0.,1.,0.));
#4880=DIRECTION('',(0.,-1.,0.));
#4881=DIRECTION('',(0.,0.,1.));
#4882=DIRECTION('center_axis',(0.,1.,0.));
#4883=DIRECTION('ref_axis',(-1.,0.,0.));
#4884=DIRECTION('',(1.,0.,0.));
#4885=DIRECTION('',(-1.,0.,0.));
#4886=DIRECTION('',(0.,0.,1.));
#4887=DIRECTION('center_axis',(1.,0.,0.));
#4888=DIRECTION('ref_axis',(0.,1.,0.));
#4889=DIRECTION('',(0.,-1.,0.));
#4890=DIRECTION('',(0.,1.,0.));
#4891=DIRECTION('center_axis',(0.,0.,1.));
#4892=DIRECTION('ref_axis',(1.,0.,0.));
#4893=DIRECTION('center_axis',(0.,0.,1.));
#4894=DIRECTION('ref_axis',(1.,0.,0.));
#4895=DIRECTION('center_axis',(0.,0.,1.));
#4896=DIRECTION('ref_axis',(1.,0.,0.));
#4897=DIRECTION('',(0.,0.,1.));
#4898=DIRECTION('center_axis',(0.,0.,-1.));
#4899=DIRECTION('ref_axis',(1.,0.,0.));
#4900=DIRECTION('center_axis',(0.,0.,1.));
#4901=DIRECTION('ref_axis',(1.,0.,0.));
#4902=DIRECTION('center_axis',(0.,0.,1.));
#4903=DIRECTION('ref_axis',(1.,0.,0.));
#4904=DIRECTION('',(0.,0.,1.));
#4905=DIRECTION('center_axis',(0.,0.,-1.));
#4906=DIRECTION('ref_axis',(1.,0.,0.));
#4907=DIRECTION('center_axis',(0.,0.,1.));
#4908=DIRECTION('ref_axis',(1.,0.,0.));
#4909=DIRECTION('center_axis',(0.,0.,1.));
#4910=DIRECTION('ref_axis',(1.,0.,0.));
#4911=DIRECTION('',(0.,0.,1.));
#4912=DIRECTION('center_axis',(0.,0.,-1.));
#4913=DIRECTION('ref_axis',(1.,0.,0.));
#4914=DIRECTION('center_axis',(0.,0.,1.));
#4915=DIRECTION('ref_axis',(1.,0.,0.));
#4916=DIRECTION('center_axis',(0.,0.,1.));
#4917=DIRECTION('ref_axis',(1.,0.,0.));
#4918=DIRECTION('',(0.,0.,1.));
#4919=DIRECTION('center_axis',(0.,0.,-1.));
#4920=DIRECTION('ref_axis',(1.,0.,0.));
#4921=DIRECTION('center_axis',(0.,0.,1.));
#4922=DIRECTION('ref_axis',(1.,0.,0.));
#4923=DIRECTION('center_axis',(0.,0.,1.));
#4924=DIRECTION('ref_axis',(1.,0.,0.));
#4925=DIRECTION('',(0.,0.,1.));
#4926=DIRECTION('center_axis',(0.,0.,-1.));
#4927=DIRECTION('ref_axis',(1.,0.,0.));
#4928=DIRECTION('center_axis',(0.,0.,1.));
#4929=DIRECTION('ref_axis',(1.,0.,0.));
#4930=DIRECTION('center_axis',(0.,0.,1.));
#4931=DIRECTION('ref_axis',(1.,0.,0.));
#4932=DIRECTION('',(0.,0.,1.));
#4933=DIRECTION('center_axis',(0.,0.,-1.));
#4934=DIRECTION('ref_axis',(1.,0.,0.));
#4935=DIRECTION('center_axis',(0.,0.,1.));
#4936=DIRECTION('ref_axis',(1.,0.,0.));
#4937=DIRECTION('center_axis',(0.,0.,1.));
#4938=DIRECTION('ref_axis',(1.,0.,0.));
#4939=DIRECTION('',(0.,0.,1.));
#4940=DIRECTION('center_axis',(0.,0.,-1.));
#4941=DIRECTION('ref_axis',(1.,0.,0.));
#4942=DIRECTION('center_axis',(0.,0.,1.));
#4943=DIRECTION('ref_axis',(1.,0.,0.));
#4944=DIRECTION('center_axis',(0.,0.,1.));
#4945=DIRECTION('ref_axis',(1.,0.,0.));
#4946=DIRECTION('',(0.,0.,1.));
#4947=DIRECTION('center_axis',(0.,0.,-1.));
#4948=DIRECTION('ref_axis',(1.,0.,0.));
#4949=DIRECTION('center_axis',(0.,0.,1.));
#4950=DIRECTION('ref_axis',(1.,0.,0.));
#4951=DIRECTION('center_axis',(0.,0.,1.));
#4952=DIRECTION('ref_axis',(1.,0.,0.));
#4953=DIRECTION('',(0.,0.,1.));
#4954=DIRECTION('center_axis',(0.,0.,-1.));
#4955=DIRECTION('ref_axis',(1.,0.,0.));
#4956=DIRECTION('center_axis',(0.,0.,1.));
#4957=DIRECTION('ref_axis',(1.,0.,0.));
#4958=DIRECTION('center_axis',(0.,0.,1.));
#4959=DIRECTION('ref_axis',(1.,0.,0.));
#4960=DIRECTION('',(0.,0.,1.));
#4961=DIRECTION('center_axis',(0.,0.,-1.));
#4962=DIRECTION('ref_axis',(1.,0.,0.));
#4963=DIRECTION('center_axis',(0.,0.,1.));
#4964=DIRECTION('ref_axis',(1.,0.,0.));
#4965=DIRECTION('center_axis',(0.,0.,1.));
#4966=DIRECTION('ref_axis',(1.,0.,0.));
#4967=DIRECTION('',(0.,0.,1.));
#4968=DIRECTION('center_axis',(0.,0.,-1.));
#4969=DIRECTION('ref_axis',(1.,0.,0.));
#4970=DIRECTION('center_axis',(0.,0.,1.));
#4971=DIRECTION('ref_axis',(1.,0.,0.));
#4972=DIRECTION('center_axis',(0.,0.,1.));
#4973=DIRECTION('ref_axis',(1.,0.,0.));
#4974=DIRECTION('',(0.,0.,1.));
#4975=DIRECTION('center_axis',(0.,0.,-1.));
#4976=DIRECTION('ref_axis',(1.,0.,0.));
#4977=DIRECTION('center_axis',(0.,1.,0.));
#4978=DIRECTION('ref_axis',(-1.,0.,0.));
#4979=DIRECTION('',(-1.,0.,0.));
#4980=DIRECTION('',(0.,0.,1.));
#4981=DIRECTION('',(-1.,0.,0.));
#4982=DIRECTION('',(0.,0.,1.));
#4983=DIRECTION('center_axis',(1.,0.,0.));
#4984=DIRECTION('ref_axis',(0.,1.,0.));
#4985=DIRECTION('',(0.,1.,0.));
#4986=DIRECTION('',(0.,1.,0.));
#4987=DIRECTION('',(0.,0.,1.));
#4988=DIRECTION('center_axis',(0.,-1.,0.));
#4989=DIRECTION('ref_axis',(1.,0.,0.));
#4990=DIRECTION('',(1.,0.,0.));
#4991=DIRECTION('',(1.,0.,0.));
#4992=DIRECTION('',(0.,0.,1.));
#4993=DIRECTION('center_axis',(-1.,0.,0.));
#4994=DIRECTION('ref_axis',(0.,-1.,0.));
#4995=DIRECTION('',(0.,-1.,0.));
#4996=DIRECTION('',(0.,-1.,0.));
#4997=DIRECTION('center_axis',(0.,0.,1.));
#4998=DIRECTION('ref_axis',(1.,0.,0.));
#4999=DIRECTION('center_axis',(0.,0.,1.));
#5000=DIRECTION('ref_axis',(1.,0.,0.));
#5001=DIRECTION('axis',(0.,0.,1.));
#5002=DIRECTION('refdir',(1.,0.,0.));
#5003=DIRECTION('center_axis',(0.,0.,1.));
#5004=DIRECTION('ref_axis',(1.,0.,0.));
#5005=DIRECTION('center_axis',(0.,0.,1.));
#5006=DIRECTION('ref_axis',(1.,0.,0.));
#5007=DIRECTION('',(0.,0.,1.));
#5008=DIRECTION('center_axis',(0.,0.,-1.));
#5009=DIRECTION('ref_axis',(1.,0.,0.));
#5010=DIRECTION('center_axis',(0.,0.,1.));
#5011=DIRECTION('ref_axis',(1.,0.,0.));
#5012=DIRECTION('center_axis',(0.,0.,1.));
#5013=DIRECTION('ref_axis',(1.,0.,0.));
#5014=DIRECTION('',(0.,0.,1.));
#5015=DIRECTION('center_axis',(0.,0.,-1.));
#5016=DIRECTION('ref_axis',(1.,0.,0.));
#5017=DIRECTION('center_axis',(0.,1.,0.));
#5018=DIRECTION('ref_axis',(-1.,0.,0.));
#5019=DIRECTION('',(-1.,0.,0.));
#5020=DIRECTION('',(0.,0.,1.));
#5021=DIRECTION('',(-1.,0.,0.));
#5022=DIRECTION('',(0.,0.,1.));
#5023=DIRECTION('center_axis',(1.,0.,0.));
#5024=DIRECTION('ref_axis',(0.,1.,0.));
#5025=DIRECTION('',(0.,1.,0.));
#5026=DIRECTION('',(0.,1.,0.));
#5027=DIRECTION('',(0.,0.,1.));
#5028=DIRECTION('center_axis',(0.,-1.,0.));
#5029=DIRECTION('ref_axis',(1.,0.,0.));
#5030=DIRECTION('',(1.,0.,0.));
#5031=DIRECTION('',(1.,0.,0.));
#5032=DIRECTION('',(0.,0.,1.));
#5033=DIRECTION('center_axis',(-1.,0.,0.));
#5034=DIRECTION('ref_axis',(0.,-1.,0.));
#5035=DIRECTION('',(0.,-1.,0.));
#5036=DIRECTION('',(0.,-1.,0.));
#5037=DIRECTION('center_axis',(0.,0.,1.));
#5038=DIRECTION('ref_axis',(1.,0.,0.));
#5039=DIRECTION('center_axis',(0.,0.,1.));
#5040=DIRECTION('ref_axis',(1.,0.,0.));
#5041=DIRECTION('axis',(0.,0.,1.));
#5042=DIRECTION('refdir',(1.,0.,0.));
#5043=DIRECTION('center_axis',(0.,1.,0.));
#5044=DIRECTION('ref_axis',(-1.,0.,0.));
#5045=DIRECTION('',(-1.,0.,0.));
#5046=DIRECTION('',(0.,0.,1.));
#5047=DIRECTION('',(-1.,0.,0.));
#5048=DIRECTION('',(0.,0.,1.));
#5049=DIRECTION('center_axis',(1.,0.,0.));
#5050=DIRECTION('ref_axis',(0.,1.,0.));
#5051=DIRECTION('',(0.,1.,0.));
#5052=DIRECTION('',(0.,1.,0.));
#5053=DIRECTION('',(0.,0.,1.));
#5054=DIRECTION('center_axis',(0.,-1.,0.));
#5055=DIRECTION('ref_axis',(1.,0.,0.));
#5056=DIRECTION('',(1.,0.,0.));
#5057=DIRECTION('',(1.,0.,0.));
#5058=DIRECTION('',(0.,0.,1.));
#5059=DIRECTION('center_axis',(-1.,0.,0.));
#5060=DIRECTION('ref_axis',(0.,-1.,0.));
#5061=DIRECTION('',(0.,-1.,0.));
#5062=DIRECTION('',(0.,-1.,0.));
#5063=DIRECTION('center_axis',(0.,0.,1.));
#5064=DIRECTION('ref_axis',(1.,0.,0.));
#5065=DIRECTION('center_axis',(0.,0.,1.));
#5066=DIRECTION('ref_axis',(1.,0.,0.));
#5067=DIRECTION('axis',(0.,0.,1.));
#5068=DIRECTION('refdir',(1.,0.,0.));
#5069=DIRECTION('center_axis',(0.,0.,1.));
#5070=DIRECTION('ref_axis',(1.,0.,0.));
#5071=DIRECTION('center_axis',(0.,0.,1.));
#5072=DIRECTION('ref_axis',(1.,0.,0.));
#5073=DIRECTION('',(0.,0.,1.));
#5074=DIRECTION('center_axis',(0.,0.,-1.));
#5075=DIRECTION('ref_axis',(1.,0.,0.));
#5076=DIRECTION('center_axis',(0.,0.,1.));
#5077=DIRECTION('ref_axis',(1.,0.,0.));
#5078=DIRECTION('center_axis',(0.,0.,1.));
#5079=DIRECTION('ref_axis',(1.,0.,0.));
#5080=DIRECTION('',(0.,0.,1.));
#5081=DIRECTION('center_axis',(0.,0.,-1.));
#5082=DIRECTION('ref_axis',(1.,0.,0.));
#5083=DIRECTION('center_axis',(0.,1.,0.));
#5084=DIRECTION('ref_axis',(-1.,0.,0.));
#5085=DIRECTION('',(-1.,0.,0.));
#5086=DIRECTION('',(0.,0.,1.));
#5087=DIRECTION('',(-1.,0.,0.));
#5088=DIRECTION('',(0.,0.,1.));
#5089=DIRECTION('center_axis',(1.,0.,0.));
#5090=DIRECTION('ref_axis',(0.,1.,0.));
#5091=DIRECTION('',(0.,1.,0.));
#5092=DIRECTION('',(0.,1.,0.));
#5093=DIRECTION('',(0.,0.,1.));
#5094=DIRECTION('center_axis',(0.,-1.,0.));
#5095=DIRECTION('ref_axis',(1.,0.,0.));
#5096=DIRECTION('',(1.,0.,0.));
#5097=DIRECTION('',(1.,0.,0.));
#5098=DIRECTION('',(0.,0.,1.));
#5099=DIRECTION('center_axis',(-1.,0.,0.));
#5100=DIRECTION('ref_axis',(0.,-1.,0.));
#5101=DIRECTION('',(0.,-1.,0.));
#5102=DIRECTION('',(0.,-1.,0.));
#5103=DIRECTION('center_axis',(0.,0.,1.));
#5104=DIRECTION('ref_axis',(1.,0.,0.));
#5105=DIRECTION('center_axis',(0.,0.,1.));
#5106=DIRECTION('ref_axis',(1.,0.,0.));
#5107=DIRECTION('axis',(0.,0.,1.));
#5108=DIRECTION('refdir',(1.,0.,0.));
#5109=DIRECTION('center_axis',(0.,1.,0.));
#5110=DIRECTION('ref_axis',(-1.,0.,0.));
#5111=DIRECTION('',(-1.,0.,0.));
#5112=DIRECTION('',(0.,0.,1.));
#5113=DIRECTION('',(-1.,0.,0.));
#5114=DIRECTION('',(0.,0.,1.));
#5115=DIRECTION('center_axis',(1.,0.,0.));
#5116=DIRECTION('ref_axis',(0.,1.,0.));
#5117=DIRECTION('',(0.,1.,0.));
#5118=DIRECTION('',(0.,1.,0.));
#5119=DIRECTION('',(0.,0.,1.));
#5120=DIRECTION('center_axis',(0.,-1.,0.));
#5121=DIRECTION('ref_axis',(1.,0.,0.));
#5122=DIRECTION('',(1.,0.,0.));
#5123=DIRECTION('',(1.,0.,0.));
#5124=DIRECTION('',(0.,0.,1.));
#5125=DIRECTION('center_axis',(-1.,0.,0.));
#5126=DIRECTION('ref_axis',(0.,-1.,0.));
#5127=DIRECTION('',(0.,-1.,0.));
#5128=DIRECTION('',(0.,-1.,0.));
#5129=DIRECTION('center_axis',(0.,0.,1.));
#5130=DIRECTION('ref_axis',(1.,0.,0.));
#5131=DIRECTION('center_axis',(0.,0.,1.));
#5132=DIRECTION('ref_axis',(1.,0.,0.));
#5133=DIRECTION('axis',(0.,0.,1.));
#5134=DIRECTION('refdir',(1.,0.,0.));
#5135=DIRECTION('center_axis',(0.,0.,1.));
#5136=DIRECTION('ref_axis',(1.,0.,0.));
#5137=DIRECTION('',(0.,0.,1.));
#5138=DIRECTION('center_axis',(0.,0.,1.));
#5139=DIRECTION('ref_axis',(1.,0.,0.));
#5140=DIRECTION('',(0.,0.,1.));
#5141=DIRECTION('center_axis',(0.,0.,-1.));
#5142=DIRECTION('ref_axis',(1.,0.,0.));
#5143=DIRECTION('center_axis',(0.,0.,1.));
#5144=DIRECTION('ref_axis',(1.,0.,0.));
#5145=DIRECTION('',(0.,0.,1.));
#5146=DIRECTION('center_axis',(0.,0.,1.));
#5147=DIRECTION('ref_axis',(1.,0.,0.));
#5148=DIRECTION('',(0.,0.,1.));
#5149=DIRECTION('center_axis',(0.,0.,-1.));
#5150=DIRECTION('ref_axis',(1.,0.,0.));
#5151=DIRECTION('center_axis',(0.,-0.707106781186547,-0.707106781186548));
#5152=DIRECTION('ref_axis',(0.,0.707106781186548,-0.707106781186547));
#5153=DIRECTION('center_axis',(0.,-1.,0.));
#5154=DIRECTION('ref_axis',(1.,0.,0.));
#5155=DIRECTION('',(1.,0.,0.));
#5156=DIRECTION('',(0.,0.,1.));
#5157=DIRECTION('',(1.,0.,0.));
#5158=DIRECTION('',(0.,0.,1.));
#5159=DIRECTION('center_axis',(1.,0.,0.));
#5160=DIRECTION('ref_axis',(0.,1.,0.));
#5161=DIRECTION('',(0.,1.,0.));
#5162=DIRECTION('',(0.,1.,0.));
#5163=DIRECTION('',(0.,0.,1.));
#5164=DIRECTION('center_axis',(0.,1.,0.));
#5165=DIRECTION('ref_axis',(-1.,0.,0.));
#5166=DIRECTION('',(-1.,0.,0.));
#5167=DIRECTION('',(-1.,0.,0.));
#5168=DIRECTION('',(0.,0.,1.));
#5169=DIRECTION('center_axis',(-1.,0.,0.));
#5170=DIRECTION('ref_axis',(0.,-1.,0.));
#5171=DIRECTION('',(0.,-1.,0.));
#5172=DIRECTION('',(0.,-1.,0.));
#5173=DIRECTION('center_axis',(0.,0.,1.));
#5174=DIRECTION('ref_axis',(1.,0.,0.));
#5175=DIRECTION('center_axis',(0.,0.,1.));
#5176=DIRECTION('ref_axis',(1.,0.,0.));
#5177=DIRECTION('center_axis',(0.,0.,-1.));
#5178=DIRECTION('ref_axis',(1.,0.,0.));
#5179=DIRECTION('',(0.,0.,1.));
#5180=DIRECTION('center_axis',(0.,0.,1.));
#5181=DIRECTION('ref_axis',(1.,0.,0.));
#5182=DIRECTION('center_axis',(0.,0.,1.));
#5183=DIRECTION('ref_axis',(1.,0.,0.));
#5184=DIRECTION('center_axis',(0.,0.,1.));
#5185=DIRECTION('ref_axis',(1.,0.,0.));
#5186=DIRECTION('center_axis',(0.,0.,1.));
#5187=DIRECTION('ref_axis',(1.,0.,0.));
#5188=DIRECTION('center_axis',(0.,0.707106781186547,-0.707106781186548));
#5189=DIRECTION('ref_axis',(0.,0.707106781186548,0.707106781186547));
#5190=DIRECTION('center_axis',(0.,0.,-1.));
#5191=DIRECTION('ref_axis',(1.,0.,0.));
#5192=DIRECTION('',(0.,0.,1.));
#5193=DIRECTION('center_axis',(0.,0.,1.));
#5194=DIRECTION('ref_axis',(1.,0.,0.));
#5195=DIRECTION('center_axis',(0.,0.,1.));
#5196=DIRECTION('ref_axis',(1.,0.,0.));
#5197=DIRECTION('center_axis',(0.,0.,1.));
#5198=DIRECTION('ref_axis',(1.,0.,0.));
#5199=DIRECTION('center_axis',(0.,-0.707106781186547,-0.707106781186548));
#5200=DIRECTION('ref_axis',(0.,0.707106781186548,-0.707106781186547));
#5201=DIRECTION('',(-1.,0.,0.));
#5202=DIRECTION('',(0.,-0.707106781186548,0.707106781186547));
#5203=DIRECTION('',(1.,0.,0.));
#5204=DIRECTION('',(0.,0.707106781186548,-0.707106781186547));
#5205=DIRECTION('',(-1.,0.,0.));
#5206=DIRECTION('center_axis',(0.,0.,1.));
#5207=DIRECTION('ref_axis',(1.,0.,0.));
#5208=DIRECTION('',(1.,0.,0.));
#5209=DIRECTION('',(0.,1.,0.));
#5210=DIRECTION('center_axis',(0.,0.707106781186547,-0.707106781186548));
#5211=DIRECTION('ref_axis',(0.,0.707106781186548,0.707106781186547));
#5212=DIRECTION('',(1.,0.,0.));
#5213=DIRECTION('',(0.,0.707106781186548,0.707106781186547));
#5214=DIRECTION('',(0.,-0.707106781186548,-0.707106781186547));
#5215=DIRECTION('',(1.,0.,0.));
#5216=DIRECTION('center_axis',(0.,0.,1.));
#5217=DIRECTION('ref_axis',(1.,0.,0.));
#5218=DIRECTION('',(-1.,0.,0.));
#5219=DIRECTION('',(0.,-1.,0.));
#5220=DIRECTION('center_axis',(0.,0.,1.));
#5221=DIRECTION('ref_axis',(1.,0.,0.));
#5222=DIRECTION('center_axis',(0.,0.,1.));
#5223=DIRECTION('ref_axis',(1.,0.,0.));
#5224=DIRECTION('',(0.,0.,1.));
#5225=DIRECTION('center_axis',(0.,0.,1.));
#5226=DIRECTION('ref_axis',(1.,0.,0.));
#5227=DIRECTION('center_axis',(0.,0.,1.));
#5228=DIRECTION('ref_axis',(1.,0.,0.));
#5229=DIRECTION('',(0.,0.,1.));
#5230=DIRECTION('center_axis',(0.,0.,1.));
#5231=DIRECTION('ref_axis',(1.,0.,0.));
#5232=DIRECTION('',(0.,-1.,0.));
#5233=DIRECTION('',(1.,0.,0.));
#5234=DIRECTION('center_axis',(0.,0.,1.));
#5235=DIRECTION('ref_axis',(1.,0.,0.));
#5236=DIRECTION('',(0.,1.,0.));
#5237=DIRECTION('',(-1.,0.,0.));
#5238=DIRECTION('center_axis',(-1.,0.,0.));
#5239=DIRECTION('ref_axis',(0.,-1.,0.));
#5240=DIRECTION('',(0.,0.,1.));
#5241=DIRECTION('',(0.,-1.,0.));
#5242=DIRECTION('',(0.,0.,1.));
#5243=DIRECTION('center_axis',(0.,1.,0.));
#5244=DIRECTION('ref_axis',(-1.,0.,0.));
#5245=DIRECTION('',(-1.,0.,0.));
#5246=DIRECTION('',(0.,0.,1.));
#5247=DIRECTION('center_axis',(1.,0.,0.));
#5248=DIRECTION('ref_axis',(0.,1.,0.));
#5249=DIRECTION('',(0.,0.,1.));
#5250=DIRECTION('',(0.,1.,0.));
#5251=DIRECTION('center_axis',(0.,-1.,0.));
#5252=DIRECTION('ref_axis',(1.,0.,0.));
#5253=DIRECTION('',(1.,0.,0.));
#5254=DIRECTION('center_axis',(0.,0.,1.));
#5255=DIRECTION('ref_axis',(1.,0.,0.));
#5256=DIRECTION('axis',(0.,0.,1.));
#5257=DIRECTION('refdir',(1.,0.,0.));
#5258=DIRECTION('center_axis',(0.,0.,1.));
#5259=DIRECTION('ref_axis',(1.,0.,0.));
#5260=DIRECTION('',(0.,0.,1.));
#5261=DIRECTION('center_axis',(0.,0.,1.));
#5262=DIRECTION('ref_axis',(1.,0.,0.));
#5263=DIRECTION('',(0.,0.,1.));
#5264=DIRECTION('center_axis',(0.,0.,-1.));
#5265=DIRECTION('ref_axis',(1.,0.,0.));
#5266=DIRECTION('center_axis',(0.,0.,1.));
#5267=DIRECTION('ref_axis',(1.,0.,0.));
#5268=DIRECTION('',(0.,0.,1.));
#5269=DIRECTION('center_axis',(0.,0.,1.));
#5270=DIRECTION('ref_axis',(1.,0.,0.));
#5271=DIRECTION('',(0.,0.,1.));
#5272=DIRECTION('center_axis',(0.,0.,-1.));
#5273=DIRECTION('ref_axis',(1.,0.,0.));
#5274=DIRECTION('center_axis',(0.,-0.707106781186547,-0.707106781186548));
#5275=DIRECTION('ref_axis',(0.,0.707106781186548,-0.707106781186547));
#5276=DIRECTION('center_axis',(0.,-1.,0.));
#5277=DIRECTION('ref_axis',(1.,0.,0.));
#5278=DIRECTION('',(1.,0.,0.));
#5279=DIRECTION('',(0.,0.,1.));
#5280=DIRECTION('',(1.,0.,0.));
#5281=DIRECTION('',(0.,0.,1.));
#5282=DIRECTION('center_axis',(1.,0.,0.));
#5283=DIRECTION('ref_axis',(0.,1.,0.));
#5284=DIRECTION('',(0.,1.,0.));
#5285=DIRECTION('',(0.,1.,0.));
#5286=DIRECTION('',(0.,0.,1.));
#5287=DIRECTION('center_axis',(0.,1.,0.));
#5288=DIRECTION('ref_axis',(-1.,0.,0.));
#5289=DIRECTION('',(-1.,0.,0.));
#5290=DIRECTION('',(-1.,0.,0.));
#5291=DIRECTION('',(0.,0.,1.));
#5292=DIRECTION('center_axis',(-1.,0.,0.));
#5293=DIRECTION('ref_axis',(0.,-1.,0.));
#5294=DIRECTION('',(0.,-1.,0.));
#5295=DIRECTION('',(0.,-1.,0.));
#5296=DIRECTION('center_axis',(0.,0.,1.));
#5297=DIRECTION('ref_axis',(1.,0.,0.));
#5298=DIRECTION('center_axis',(0.,0.,1.));
#5299=DIRECTION('ref_axis',(1.,0.,0.));
#5300=DIRECTION('center_axis',(0.,0.,-1.));
#5301=DIRECTION('ref_axis',(1.,0.,0.));
#5302=DIRECTION('',(0.,0.,1.));
#5303=DIRECTION('center_axis',(0.,0.,1.));
#5304=DIRECTION('ref_axis',(1.,0.,0.));
#5305=DIRECTION('center_axis',(0.,0.,1.));
#5306=DIRECTION('ref_axis',(1.,0.,0.));
#5307=DIRECTION('center_axis',(0.,0.,1.));
#5308=DIRECTION('ref_axis',(1.,0.,0.));
#5309=DIRECTION('center_axis',(0.,0.,1.));
#5310=DIRECTION('ref_axis',(1.,0.,0.));
#5311=DIRECTION('center_axis',(0.,0.707106781186547,-0.707106781186548));
#5312=DIRECTION('ref_axis',(0.,0.707106781186548,0.707106781186547));
#5313=DIRECTION('center_axis',(0.,0.,-1.));
#5314=DIRECTION('ref_axis',(1.,0.,0.));
#5315=DIRECTION('',(0.,0.,1.));
#5316=DIRECTION('center_axis',(0.,0.,1.));
#5317=DIRECTION('ref_axis',(1.,0.,0.));
#5318=DIRECTION('center_axis',(0.,0.,1.));
#5319=DIRECTION('ref_axis',(1.,0.,0.));
#5320=DIRECTION('center_axis',(0.,0.,1.));
#5321=DIRECTION('ref_axis',(1.,0.,0.));
#5322=DIRECTION('center_axis',(0.,-0.707106781186547,-0.707106781186548));
#5323=DIRECTION('ref_axis',(0.,0.707106781186548,-0.707106781186547));
#5324=DIRECTION('',(-1.,0.,0.));
#5325=DIRECTION('',(0.,-0.707106781186548,0.707106781186547));
#5326=DIRECTION('',(1.,0.,0.));
#5327=DIRECTION('',(0.,0.707106781186548,-0.707106781186547));
#5328=DIRECTION('',(-1.,0.,0.));
#5329=DIRECTION('center_axis',(0.,0.,1.));
#5330=DIRECTION('ref_axis',(1.,0.,0.));
#5331=DIRECTION('',(1.,0.,0.));
#5332=DIRECTION('',(0.,1.,0.));
#5333=DIRECTION('center_axis',(0.,0.707106781186547,-0.707106781186548));
#5334=DIRECTION('ref_axis',(0.,0.707106781186548,0.707106781186547));
#5335=DIRECTION('',(1.,0.,0.));
#5336=DIRECTION('',(0.,0.707106781186548,0.707106781186547));
#5337=DIRECTION('',(0.,-0.707106781186548,-0.707106781186547));
#5338=DIRECTION('',(1.,0.,0.));
#5339=DIRECTION('center_axis',(0.,0.,1.));
#5340=DIRECTION('ref_axis',(1.,0.,0.));
#5341=DIRECTION('',(-1.,0.,0.));
#5342=DIRECTION('',(0.,-1.,0.));
#5343=DIRECTION('center_axis',(0.,0.,1.));
#5344=DIRECTION('ref_axis',(1.,0.,0.));
#5345=DIRECTION('center_axis',(0.,0.,1.));
#5346=DIRECTION('ref_axis',(1.,0.,0.));
#5347=DIRECTION('',(0.,0.,1.));
#5348=DIRECTION('center_axis',(0.,0.,1.));
#5349=DIRECTION('ref_axis',(1.,0.,0.));
#5350=DIRECTION('center_axis',(0.,0.,1.));
#5351=DIRECTION('ref_axis',(1.,0.,0.));
#5352=DIRECTION('',(0.,0.,1.));
#5353=DIRECTION('center_axis',(0.,0.,1.));
#5354=DIRECTION('ref_axis',(1.,0.,0.));
#5355=DIRECTION('',(0.,-1.,0.));
#5356=DIRECTION('',(1.,0.,0.));
#5357=DIRECTION('center_axis',(0.,0.,1.));
#5358=DIRECTION('ref_axis',(1.,0.,0.));
#5359=DIRECTION('',(0.,1.,0.));
#5360=DIRECTION('',(-1.,0.,0.));
#5361=DIRECTION('center_axis',(-1.,0.,0.));
#5362=DIRECTION('ref_axis',(0.,-1.,0.));
#5363=DIRECTION('',(0.,0.,1.));
#5364=DIRECTION('',(0.,-1.,0.));
#5365=DIRECTION('',(0.,0.,1.));
#5366=DIRECTION('center_axis',(0.,1.,0.));
#5367=DIRECTION('ref_axis',(-1.,0.,0.));
#5368=DIRECTION('',(-1.,0.,0.));
#5369=DIRECTION('',(0.,0.,1.));
#5370=DIRECTION('center_axis',(1.,0.,0.));
#5371=DIRECTION('ref_axis',(0.,1.,0.));
#5372=DIRECTION('',(0.,0.,1.));
#5373=DIRECTION('',(0.,1.,0.));
#5374=DIRECTION('center_axis',(0.,-1.,0.));
#5375=DIRECTION('ref_axis',(1.,0.,0.));
#5376=DIRECTION('',(1.,0.,0.));
#5377=DIRECTION('center_axis',(0.,0.,1.));
#5378=DIRECTION('ref_axis',(1.,0.,0.));
#5379=DIRECTION('axis',(0.,0.,1.));
#5380=DIRECTION('refdir',(1.,0.,0.));
#5381=DIRECTION('center_axis',(1.,0.,0.));
#5382=DIRECTION('ref_axis',(0.,0.,-1.));
#5383=DIRECTION('center_axis',(1.,0.,0.));
#5384=DIRECTION('ref_axis',(0.,0.,-1.));
#5385=DIRECTION('',(1.,0.,0.));
#5386=DIRECTION('center_axis',(-1.,0.,0.));
#5387=DIRECTION('ref_axis',(0.,0.,-1.));
#5388=DIRECTION('center_axis',(0.,0.,1.));
#5389=DIRECTION('ref_axis',(1.,0.,0.));
#5390=DIRECTION('',(0.,0.,1.));
#5391=DIRECTION('center_axis',(0.,0.,-1.));
#5392=DIRECTION('ref_axis',(1.,0.,0.));
#5393=DIRECTION('',(0.,0.,1.));
#5394=DIRECTION('center_axis',(0.,0.,1.));
#5395=DIRECTION('ref_axis',(1.,0.,0.));
#5396=DIRECTION('center_axis',(0.,0.,1.));
#5397=DIRECTION('ref_axis',(1.,0.,0.));
#5398=DIRECTION('',(0.,0.,1.));
#5399=DIRECTION('center_axis',(0.,0.,1.));
#5400=DIRECTION('ref_axis',(1.,0.,0.));
#5401=DIRECTION('',(0.,0.,1.));
#5402=DIRECTION('center_axis',(0.,0.,-1.));
#5403=DIRECTION('ref_axis',(1.,0.,0.));
#5404=DIRECTION('center_axis',(0.,0.,1.));
#5405=DIRECTION('ref_axis',(1.,0.,0.));
#5406=DIRECTION('center_axis',(0.,0.,1.));
#5407=DIRECTION('ref_axis',(1.,0.,0.));
#5408=DIRECTION('center_axis',(0.,0.,1.));
#5409=DIRECTION('ref_axis',(1.,0.,0.));
#5410=DIRECTION('',(0.,0.,1.));
#5411=DIRECTION('center_axis',(0.,0.,-1.));
#5412=DIRECTION('ref_axis',(1.,0.,0.));
#5413=DIRECTION('',(0.,0.,1.));
#5414=DIRECTION('center_axis',(0.,0.,1.));
#5415=DIRECTION('ref_axis',(1.,0.,0.));
#5416=DIRECTION('center_axis',(0.,0.,1.));
#5417=DIRECTION('ref_axis',(1.,0.,0.));
#5418=DIRECTION('',(0.,0.,1.));
#5419=DIRECTION('center_axis',(0.,0.,1.));
#5420=DIRECTION('ref_axis',(1.,0.,0.));
#5421=DIRECTION('',(0.,0.,1.));
#5422=DIRECTION('center_axis',(0.,0.,-1.));
#5423=DIRECTION('ref_axis',(1.,0.,0.));
#5424=DIRECTION('center_axis',(0.,0.,1.));
#5425=DIRECTION('ref_axis',(1.,0.,0.));
#5426=DIRECTION('center_axis',(0.,0.,1.));
#5427=DIRECTION('ref_axis',(1.,0.,0.));
#5428=DIRECTION('center_axis',(0.,0.,1.));
#5429=DIRECTION('ref_axis',(1.,0.,0.));
#5430=DIRECTION('',(0.,1.,0.));
#5431=DIRECTION('',(-1.,0.,0.));
#5432=DIRECTION('',(0.,-1.,0.));
#5433=DIRECTION('center_axis',(0.,0.,1.));
#5434=DIRECTION('ref_axis',(1.,0.,0.));
#5435=DIRECTION('',(0.,1.,0.));
#5436=DIRECTION('',(0.,-1.,0.));
#5437=DIRECTION('center_axis',(0.,0.,1.));
#5438=DIRECTION('ref_axis',(1.,0.,0.));
#5439=DIRECTION('',(0.,-1.,0.));
#5440=DIRECTION('',(1.,0.,0.));
#5441=DIRECTION('',(0.,1.,0.));
#5442=DIRECTION('center_axis',(0.,0.,1.));
#5443=DIRECTION('ref_axis',(1.,0.,0.));
#5444=DIRECTION('center_axis',(0.,0.,1.));
#5445=DIRECTION('ref_axis',(1.,0.,0.));
#5446=DIRECTION('',(0.,0.,1.));
#5447=DIRECTION('center_axis',(0.,0.,1.));
#5448=DIRECTION('ref_axis',(1.,0.,0.));
#5449=DIRECTION('center_axis',(0.,0.,1.));
#5450=DIRECTION('ref_axis',(1.,0.,0.));
#5451=DIRECTION('',(0.,0.,1.));
#5452=DIRECTION('center_axis',(0.,1.,0.));
#5453=DIRECTION('ref_axis',(-1.,0.,0.));
#5454=DIRECTION('',(-1.,0.,0.));
#5455=DIRECTION('',(0.,0.,1.));
#5456=DIRECTION('',(0.,0.,1.));
#5457=DIRECTION('center_axis',(1.,0.,0.));
#5458=DIRECTION('ref_axis',(0.,1.,0.));
#5459=DIRECTION('',(0.,1.,0.));
#5460=DIRECTION('',(0.,0.,1.));
#5461=DIRECTION('center_axis',(0.,-1.,0.));
#5462=DIRECTION('ref_axis',(1.,0.,0.));
#5463=DIRECTION('',(1.,0.,0.));
#5464=DIRECTION('',(0.,0.,1.));
#5465=DIRECTION('center_axis',(-1.,0.,0.));
#5466=DIRECTION('ref_axis',(0.,-1.,0.));
#5467=DIRECTION('',(0.,-1.,0.));
#5468=DIRECTION('center_axis',(0.,0.,1.));
#5469=DIRECTION('ref_axis',(1.,0.,0.));
#5470=DIRECTION('axis',(0.,0.,1.));
#5471=DIRECTION('refdir',(1.,0.,0.));
#5472=DIRECTION('center_axis',(1.,0.,0.));
#5473=DIRECTION('ref_axis',(0.,0.,-1.));
#5474=DIRECTION('',(0.,-0.707106781186547,-0.707106781186548));
#5475=DIRECTION('',(0.,-1.,0.));
#5476=DIRECTION('',(0.,-0.707106781186547,0.707106781186548));
#5477=DIRECTION('',(0.,0.,1.));
#5478=DIRECTION('',(0.,0.707106781186547,0.707106781186548));
#5479=DIRECTION('',(0.,1.,0.));
#5480=DIRECTION('',(0.,0.707106781186547,-0.707106781186548));
#5481=DIRECTION('',(0.,0.,-1.));
#5482=DIRECTION('center_axis',(0.,0.707106781186548,-0.707106781186547));
#5483=DIRECTION('ref_axis',(-1.,0.,0.));
#5484=DIRECTION('',(1.,0.,0.));
#5485=DIRECTION('',(0.,-0.707106781186547,-0.707106781186548));
#5486=DIRECTION('',(-1.,0.,0.));
#5487=DIRECTION('center_axis',(0.,1.,0.));
#5488=DIRECTION('ref_axis',(-1.,0.,0.));
#5489=DIRECTION('',(-1.,0.,0.));
#5490=DIRECTION('',(0.,0.,-1.));
#5491=DIRECTION('center_axis',(0.,0.707106781186548,0.707106781186547));
#5492=DIRECTION('ref_axis',(1.,0.,0.));
#5493=DIRECTION('',(1.,0.,0.));
#5494=DIRECTION('',(0.,0.707106781186547,-0.707106781186548));
#5495=DIRECTION('center_axis',(0.,0.,1.));
#5496=DIRECTION('ref_axis',(1.,0.,0.));
#5497=DIRECTION('',(-1.,0.,0.));
#5498=DIRECTION('',(0.,1.,0.));
#5499=DIRECTION('center_axis',(1.,0.,0.));
#5500=DIRECTION('ref_axis',(0.,0.,-1.));
#5501=DIRECTION('',(0.,-0.707106781186547,0.707106781186548));
#5502=DIRECTION('',(0.,-1.,0.));
#5503=DIRECTION('',(0.,0.707106781186547,0.707106781186548));
#5504=DIRECTION('',(0.,0.,1.));
#5505=DIRECTION('center_axis',(0.,0.,1.));
#5506=DIRECTION('ref_axis',(1.,0.,0.));
#5507=DIRECTION('',(1.,0.,0.));
#5508=DIRECTION('center_axis',(0.,-0.707106781186548,0.707106781186547));
#5509=DIRECTION('ref_axis',(1.,0.,0.));
#5510=DIRECTION('',(1.,0.,0.));
#5511=DIRECTION('center_axis',(0.,-0.707106781186548,-0.707106781186547));
#5512=DIRECTION('ref_axis',(-1.,0.,0.));
#5513=DIRECTION('',(-1.,0.,0.));
#5514=DIRECTION('center_axis',(0.,-1.,0.));
#5515=DIRECTION('ref_axis',(1.,0.,0.));
#5516=DIRECTION('axis',(0.,0.,1.));
#5517=DIRECTION('refdir',(1.,0.,0.));
#5518=DIRECTION('center_axis',(0.,1.,0.));
#5519=DIRECTION('ref_axis',(0.,0.,1.));
#5520=DIRECTION('center_axis',(0.,-1.,0.));
#5521=DIRECTION('ref_axis',(1.,0.,0.));
#5522=DIRECTION('center_axis',(0.,-1.,0.));
#5523=DIRECTION('ref_axis',(1.,0.,0.));
#5524=DIRECTION('center_axis',(0.,-1.,0.));
#5525=DIRECTION('ref_axis',(1.,0.,0.));
#5526=DIRECTION('',(0.707106781186548,0.707106781186547,8.65956056235494E-17));
#5527=DIRECTION('center_axis',(0.,-1.,0.));
#5528=DIRECTION('ref_axis',(1.,0.,0.));
#5529=DIRECTION('center_axis',(0.,-1.,0.));
#5530=DIRECTION('ref_axis',(1.,0.,0.));
#5531=DIRECTION('',(0.,1.,0.));
#5532=DIRECTION('center_axis',(0.,1.,0.));
#5533=DIRECTION('ref_axis',(1.,0.,0.));
#5534=DIRECTION('center_axis',(0.,-1.,0.));
#5535=DIRECTION('ref_axis',(1.,0.,0.));
#5536=DIRECTION('',(-0.707106781186547,0.707106781186548,-8.65956056235493E-17));
#5537=DIRECTION('center_axis',(0.,-1.,0.));
#5538=DIRECTION('ref_axis',(0.,0.,-1.));
#5539=DIRECTION('center_axis',(0.,-1.,0.));
#5540=DIRECTION('ref_axis',(1.,0.,0.));
#5541=DIRECTION('center_axis',(0.,1.,0.));
#5542=DIRECTION('ref_axis',(1.,0.,0.));
#5543=DIRECTION('center_axis',(0.,1.,0.));
#5544=DIRECTION('ref_axis',(1.,0.,0.));
#5545=DIRECTION('',(-0.447213595499958,0.894427190999916,-5.47678698264203E-17));
#5546=DIRECTION('center_axis',(0.,-1.,0.));
#5547=DIRECTION('ref_axis',(1.,0.,0.));
#5548=DIRECTION('center_axis',(0.,1.,0.));
#5549=DIRECTION('ref_axis',(1.,0.,0.));
#5550=DIRECTION('',(0.,1.,0.));
#5551=DIRECTION('center_axis',(0.,1.,0.));
#5552=DIRECTION('ref_axis',(1.,0.,0.));
#5553=DIRECTION('center_axis',(0.,-1.,0.));
#5554=DIRECTION('ref_axis',(1.,0.,0.));
#5555=DIRECTION('',(-0.707106781186547,0.707106781186548,-8.65956056235493E-17));
#5556=DIRECTION('center_axis',(0.,-1.,0.));
#5557=DIRECTION('ref_axis',(0.,0.,-1.));
#5558=DIRECTION('center_axis',(0.866025403784439,0.,-0.5));
#5559=DIRECTION('ref_axis',(0.5,0.,0.866025403784439));
#5560=DIRECTION('',(-0.5,0.,-0.866025403784439));
#5561=DIRECTION('',(0.,-1.,0.));
#5562=DIRECTION('',(0.5,0.,0.866025403784439));
#5563=DIRECTION('',(0.,-1.,0.));
#5564=DIRECTION('center_axis',(1.92296268638356E-16,0.,-1.));
#5565=DIRECTION('ref_axis',(1.,0.,1.92296268638356E-16));
#5566=DIRECTION('',(-1.,0.,-1.92296268638356E-16));
#5567=DIRECTION('',(0.,-1.,0.));
#5568=DIRECTION('',(1.,0.,1.92296268638356E-16));
#5569=DIRECTION('center_axis',(-0.866025403784439,0.,-0.5));
#5570=DIRECTION('ref_axis',(0.5,0.,-0.866025403784439));
#5571=DIRECTION('',(-0.5,0.,0.866025403784438));
#5572=DIRECTION('',(0.,-1.,0.));
#5573=DIRECTION('',(0.5,0.,-0.866025403784438));
#5574=DIRECTION('center_axis',(-0.866025403784439,0.,0.5));
#5575=DIRECTION('ref_axis',(-0.5,0.,-0.866025403784439));
#5576=DIRECTION('',(0.5,0.,0.866025403784439));
#5577=DIRECTION('',(0.,-1.,0.));
#5578=DIRECTION('',(-0.5,0.,-0.866025403784439));
#5579=DIRECTION('center_axis',(-1.92296268638356E-16,0.,1.));
#5580=DIRECTION('ref_axis',(-1.,0.,-1.92296268638356E-16));
#5581=DIRECTION('',(1.,0.,1.92296268638356E-16));
#5582=DIRECTION('',(0.,-1.,0.));
#5583=DIRECTION('',(-1.,0.,-1.92296268638356E-16));
#5584=DIRECTION('center_axis',(0.866025403784439,0.,0.5));
#5585=DIRECTION('ref_axis',(-0.5,0.,0.866025403784439));
#5586=DIRECTION('',(0.5,0.,-0.866025403784439));
#5587=DIRECTION('',(-0.5,0.,0.866025403784439));
#5588=DIRECTION('center_axis',(0.,1.,0.));
#5589=DIRECTION('ref_axis',(1.,0.,0.));
#5590=DIRECTION('center_axis',(0.,-1.,0.));
#5591=DIRECTION('ref_axis',(0.,0.,-1.));
#5592=DIRECTION('axis',(0.,0.,1.));
#5593=DIRECTION('refdir',(1.,0.,0.));
#5594=DIRECTION('center_axis',(0.,1.,0.));
#5595=DIRECTION('ref_axis',(0.,0.,1.));
#5596=DIRECTION('center_axis',(0.,-1.,0.));
#5597=DIRECTION('ref_axis',(1.,0.,0.));
#5598=DIRECTION('center_axis',(0.,-1.,0.));
#5599=DIRECTION('ref_axis',(1.,0.,0.));
#5600=DIRECTION('center_axis',(0.,-1.,0.));
#5601=DIRECTION('ref_axis',(1.,0.,0.));
#5602=DIRECTION('',(0.707106781186548,0.707106781186547,8.65956056235493E-17));
#5603=DIRECTION('center_axis',(0.,-1.,0.));
#5604=DIRECTION('ref_axis',(1.,0.,0.));
#5605=DIRECTION('center_axis',(0.,-1.,0.));
#5606=DIRECTION('ref_axis',(1.,0.,0.));
#5607=DIRECTION('',(0.,1.,0.));
#5608=DIRECTION('center_axis',(0.,1.,0.));
#5609=DIRECTION('ref_axis',(1.,0.,0.));
#5610=DIRECTION('center_axis',(0.,-1.,0.));
#5611=DIRECTION('ref_axis',(1.,0.,0.));
#5612=DIRECTION('',(-0.707106781186547,0.707106781186548,-8.65956056235493E-17));
#5613=DIRECTION('center_axis',(0.,-1.,0.));
#5614=DIRECTION('ref_axis',(0.,0.,-1.));
#5615=DIRECTION('center_axis',(0.,-1.,0.));
#5616=DIRECTION('ref_axis',(1.,0.,0.));
#5617=DIRECTION('center_axis',(0.,1.,0.));
#5618=DIRECTION('ref_axis',(1.,0.,0.));
#5619=DIRECTION('center_axis',(0.,1.,0.));
#5620=DIRECTION('ref_axis',(1.,0.,0.));
#5621=DIRECTION('',(-0.447213595499958,0.894427190999916,-5.47678698264203E-17));
#5622=DIRECTION('center_axis',(0.,-1.,0.));
#5623=DIRECTION('ref_axis',(1.,0.,0.));
#5624=DIRECTION('center_axis',(0.,1.,0.));
#5625=DIRECTION('ref_axis',(1.,0.,0.));
#5626=DIRECTION('',(0.,1.,0.));
#5627=DIRECTION('center_axis',(0.,1.,0.));
#5628=DIRECTION('ref_axis',(1.,0.,0.));
#5629=DIRECTION('center_axis',(0.,-1.,0.));
#5630=DIRECTION('ref_axis',(1.,0.,0.));
#5631=DIRECTION('',(-0.707106781186547,0.707106781186548,-8.65956056235493E-17));
#5632=DIRECTION('center_axis',(0.,-1.,0.));
#5633=DIRECTION('ref_axis',(0.,0.,-1.));
#5634=DIRECTION('center_axis',(0.866025403784439,0.,-0.5));
#5635=DIRECTION('ref_axis',(0.5,0.,0.866025403784439));
#5636=DIRECTION('',(-0.5,0.,-0.866025403784439));
#5637=DIRECTION('',(0.,-1.,0.));
#5638=DIRECTION('',(0.5,0.,0.866025403784439));
#5639=DIRECTION('',(0.,-1.,0.));
#5640=DIRECTION('center_axis',(1.20185167898973E-16,0.,-1.));
#5641=DIRECTION('ref_axis',(1.,0.,1.20185167898973E-16));
#5642=DIRECTION('',(-1.,0.,-1.20185167898973E-16));
#5643=DIRECTION('',(0.,-1.,0.));
#5644=DIRECTION('',(1.,0.,1.20185167898973E-16));
#5645=DIRECTION('center_axis',(-0.866025403784439,0.,-0.5));
#5646=DIRECTION('ref_axis',(0.5,0.,-0.866025403784439));
#5647=DIRECTION('',(-0.5,0.,0.866025403784439));
#5648=DIRECTION('',(0.,-1.,0.));
#5649=DIRECTION('',(0.5,0.,-0.866025403784439));
#5650=DIRECTION('center_axis',(-0.866025403784439,0.,0.5));
#5651=DIRECTION('ref_axis',(-0.5,0.,-0.866025403784439));
#5652=DIRECTION('',(0.5,0.,0.866025403784439));
#5653=DIRECTION('',(0.,-1.,0.));
#5654=DIRECTION('',(-0.5,0.,-0.866025403784439));
#5655=DIRECTION('center_axis',(-2.40370335797945E-16,0.,1.));
#5656=DIRECTION('ref_axis',(-1.,0.,-2.40370335797945E-16));
#5657=DIRECTION('',(1.,0.,2.40370335797945E-16));
#5658=DIRECTION('',(0.,-1.,0.));
#5659=DIRECTION('',(-1.,0.,-2.40370335797945E-16));
#5660=DIRECTION('center_axis',(0.866025403784439,0.,0.5));
#5661=DIRECTION('ref_axis',(-0.5,0.,0.866025403784439));
#5662=DIRECTION('',(0.5,0.,-0.866025403784439));
#5663=DIRECTION('',(-0.5,0.,0.866025403784439));
#5664=DIRECTION('center_axis',(0.,1.,0.));
#5665=DIRECTION('ref_axis',(1.,0.,0.));
#5666=DIRECTION('center_axis',(0.,-1.,0.));
#5667=DIRECTION('ref_axis',(0.,0.,-1.));
#5668=DIRECTION('axis',(0.,0.,1.));
#5669=DIRECTION('refdir',(1.,0.,0.));
#5670=DIRECTION('center_axis',(0.,1.,0.));
#5671=DIRECTION('ref_axis',(1.,0.,0.));
#5672=DIRECTION('center_axis',(0.,-1.,0.));
#5673=DIRECTION('ref_axis',(1.,0.,0.));
#5674=DIRECTION('',(0.,-1.,0.));
#5675=DIRECTION('center_axis',(0.,-1.,0.));
#5676=DIRECTION('ref_axis',(1.,0.,0.));
#5677=DIRECTION('center_axis',(0.,1.,0.));
#5678=DIRECTION('ref_axis',(1.,0.,0.));
#5679=DIRECTION('center_axis',(0.,1.,0.));
#5680=DIRECTION('ref_axis',(1.,0.,0.));
#5681=DIRECTION('',(0.,-1.,0.));
#5682=DIRECTION('center_axis',(0.,1.,0.));
#5683=DIRECTION('ref_axis',(1.,0.,0.));
#5684=DIRECTION('center_axis',(0.,1.,0.));
#5685=DIRECTION('ref_axis',(1.,0.,0.));
#5686=DIRECTION('center_axis',(0.,1.,0.));
#5687=DIRECTION('ref_axis',(1.,0.,0.));
#5688=DIRECTION('axis',(0.,0.,1.));
#5689=DIRECTION('refdir',(1.,0.,0.));
#5690=DIRECTION('center_axis',(0.,1.,0.));
#5691=DIRECTION('ref_axis',(1.,0.,0.));
#5692=DIRECTION('',(0.866025403784439,-0.5,1.06057523872491E-16));
#5693=DIRECTION('center_axis',(0.,-1.,0.));
#5694=DIRECTION('ref_axis',(1.,0.,0.));
#5695=DIRECTION('center_axis',(0.,-1.,0.));
#5696=DIRECTION('ref_axis',(1.,0.,0.));
#5697=DIRECTION('center_axis',(0.,1.,0.));
#5698=DIRECTION('ref_axis',(1.,0.,0.));
#5699=DIRECTION('',(-0.866025403784439,-0.5,-1.06057523872491E-16));
#5700=DIRECTION('center_axis',(1.20185167898973E-16,0.,-1.));
#5701=DIRECTION('ref_axis',(-1.,0.,-1.20185167898973E-16));
#5702=DIRECTION('',(0.,1.,0.));
#5703=DIRECTION('',(0.,1.,0.));
#5704=DIRECTION('center_axis',(-0.866025403784439,0.,-0.5));
#5705=DIRECTION('ref_axis',(-0.5,0.,0.866025403784439));
#5706=DIRECTION('',(0.,1.,0.));
#5707=DIRECTION('center_axis',(-0.866025403784439,0.,0.5));
#5708=DIRECTION('ref_axis',(0.5,0.,0.866025403784439));
#5709=DIRECTION('',(0.,1.,0.));
#5710=DIRECTION('center_axis',(0.,1.,0.));
#5711=DIRECTION('ref_axis',(1.,0.,0.));
#5712=DIRECTION('center_axis',(0.,1.,0.));
#5713=DIRECTION('ref_axis',(1.,0.,0.));
#5714=DIRECTION('',(0.,-1.,0.));
#5715=DIRECTION('center_axis',(0.,1.,0.));
#5716=DIRECTION('ref_axis',(1.,0.,0.));
#5717=DIRECTION('center_axis',(-2.40370335797945E-16,0.,1.));
#5718=DIRECTION('ref_axis',(1.,0.,2.40370335797945E-16));
#5719=DIRECTION('',(0.,1.,0.));
#5720=DIRECTION('center_axis',(0.866025403784439,0.,-0.5));
#5721=DIRECTION('ref_axis',(-0.5,0.,-0.866025403784439));
#5722=DIRECTION('',(0.,1.,0.));
#5723=DIRECTION('center_axis',(0.866025403784439,0.,0.5));
#5724=DIRECTION('ref_axis',(0.5,0.,-0.866025403784439));
#5725=DIRECTION('center_axis',(0.,1.,0.));
#5726=DIRECTION('ref_axis',(1.,0.,0.));
#5727=DIRECTION('center_axis',(0.,1.,0.));
#5728=DIRECTION('ref_axis',(1.,0.,0.));
#5729=DIRECTION('',(0.,0.,1.));
#5730=DIRECTION('',(1.,0.,0.));
#5731=DIRECTION('',(0.,0.,1.));
#5732=DIRECTION('',(1.,0.,0.));
#5733=DIRECTION('',(0.,0.,1.));
#5734=DIRECTION('',(1.,0.,0.));
#5735=DIRECTION('',(0.,0.,1.));
#5736=DIRECTION('',(1.,0.,0.));
#5737=DIRECTION('',(0.,0.,1.));
#5738=DIRECTION('',(1.,0.,0.));
#5739=DIRECTION('',(0.,0.,1.));
#5740=DIRECTION('',(1.,0.,0.));
#5741=DIRECTION('',(0.,0.,1.));
#5742=DIRECTION('',(1.,0.,0.));
#5743=DIRECTION('',(0.,0.,1.));
#5744=DIRECTION('',(1.,0.,0.));
#5745=DIRECTION('',(0.,-1.,2.22044604925031E-16));
#5746=DIRECTION('',(1.,0.,0.));
#5747=DIRECTION('',(0.,-1.,2.22044604925031E-16));
#5748=DIRECTION('',(1.,0.,0.));
#5749=DIRECTION('',(0.,-1.,2.22044604925031E-16));
#5750=DIRECTION('',(1.,0.,0.));
#5751=DIRECTION('',(0.,-1.,2.22044604925031E-16));
#5752=DIRECTION('',(1.,0.,0.));
#5753=DIRECTION('',(0.,-1.,2.22044604925031E-16));
#5754=DIRECTION('',(1.,0.,0.));
#5755=DIRECTION('',(0.,-1.,2.22044604925031E-16));
#5756=DIRECTION('',(1.,0.,0.));
#5757=DIRECTION('',(0.,0.,1.));
#5758=DIRECTION('',(1.,0.,0.));
#5759=DIRECTION('',(0.,-1.,2.22044604925031E-16));
#5760=DIRECTION('',(1.,0.,0.));
#5761=DIRECTION('',(0.,-1.,2.22044604925031E-16));
#5762=DIRECTION('',(1.,0.,0.));
#5763=DIRECTION('',(0.,0.,1.));
#5764=DIRECTION('',(1.,0.,0.));
#5765=DIRECTION('',(0.,-1.,2.22044604925031E-16));
#5766=DIRECTION('',(1.,0.,0.));
#5767=DIRECTION('',(0.,-1.,2.22044604925031E-16));
#5768=DIRECTION('',(1.,0.,0.));
#5769=DIRECTION('',(0.,0.,1.));
#5770=DIRECTION('',(2.22044604925031E-16,1.,0.));
#5771=DIRECTION('',(0.,0.,1.));
#5772=DIRECTION('',(2.22044604925031E-16,1.,0.));
#5773=DIRECTION('',(0.,0.,1.));
#5774=DIRECTION('',(2.22044604925031E-16,1.,0.));
#5775=DIRECTION('axis',(0.,0.,1.));
#5776=DIRECTION('refdir',(1.,0.,0.));
#5777=DIRECTION('axis',(0.,0.,1.));
#5778=DIRECTION('refdir',(1.,0.,0.));
#5779=DIRECTION('center_axis',(0.,0.,1.));
#5780=DIRECTION('ref_axis',(1.,0.,0.));
#5781=DIRECTION('center_axis',(0.,0.,1.));
#5782=DIRECTION('ref_axis',(1.,0.,0.));
#5783=DIRECTION('',(0.,0.,1.));
#5784=DIRECTION('center_axis',(0.,0.,-1.));
#5785=DIRECTION('ref_axis',(1.,0.,0.));
#5786=DIRECTION('center_axis',(0.,0.,1.));
#5787=DIRECTION('ref_axis',(1.,0.,0.));
#5788=DIRECTION('center_axis',(0.,0.,1.));
#5789=DIRECTION('ref_axis',(1.,0.,0.));
#5790=DIRECTION('',(0.,0.,1.));
#5791=DIRECTION('center_axis',(0.,0.,-1.));
#5792=DIRECTION('ref_axis',(1.,0.,0.));
#5793=DIRECTION('center_axis',(0.,0.,1.));
#5794=DIRECTION('ref_axis',(1.,0.,0.));
#5795=DIRECTION('center_axis',(0.,0.,1.));
#5796=DIRECTION('ref_axis',(1.,0.,0.));
#5797=DIRECTION('',(0.,0.,1.));
#5798=DIRECTION('center_axis',(0.,0.,-1.));
#5799=DIRECTION('ref_axis',(1.,0.,0.));
#5800=DIRECTION('center_axis',(0.,0.,1.));
#5801=DIRECTION('ref_axis',(1.,0.,0.));
#5802=DIRECTION('center_axis',(0.,0.,1.));
#5803=DIRECTION('ref_axis',(1.,0.,0.));
#5804=DIRECTION('',(0.,0.,1.));
#5805=DIRECTION('center_axis',(0.,0.,-1.));
#5806=DIRECTION('ref_axis',(1.,0.,0.));
#5807=DIRECTION('center_axis',(0.,1.,0.));
#5808=DIRECTION('ref_axis',(-1.,0.,0.));
#5809=DIRECTION('',(-1.,0.,0.));
#5810=DIRECTION('',(0.,0.,1.));
#5811=DIRECTION('',(-1.,0.,0.));
#5812=DIRECTION('',(0.,0.,1.));
#5813=DIRECTION('center_axis',(1.,0.,0.));
#5814=DIRECTION('ref_axis',(0.,1.,0.));
#5815=DIRECTION('',(0.,1.,0.));
#5816=DIRECTION('',(0.,1.,0.));
#5817=DIRECTION('',(0.,0.,1.));
#5818=DIRECTION('center_axis',(0.,-1.,0.));
#5819=DIRECTION('ref_axis',(1.,0.,0.));
#5820=DIRECTION('',(1.,0.,0.));
#5821=DIRECTION('',(1.,0.,0.));
#5822=DIRECTION('',(0.,0.,1.));
#5823=DIRECTION('center_axis',(-1.,0.,0.));
#5824=DIRECTION('ref_axis',(0.,-1.,0.));
#5825=DIRECTION('',(0.,-1.,0.));
#5826=DIRECTION('',(0.,-1.,0.));
#5827=DIRECTION('center_axis',(0.,0.,1.));
#5828=DIRECTION('ref_axis',(1.,0.,0.));
#5829=DIRECTION('center_axis',(0.,0.,1.));
#5830=DIRECTION('ref_axis',(1.,0.,0.));
#5831=DIRECTION('axis',(0.,0.,1.));
#5832=DIRECTION('refdir',(1.,0.,0.));
#5833=DIRECTION('center_axis',(0.,0.,1.));
#5834=DIRECTION('ref_axis',(1.,0.,0.));
#5835=DIRECTION('center_axis',(0.,0.,1.));
#5836=DIRECTION('ref_axis',(1.,0.,0.));
#5837=DIRECTION('',(0.,0.,1.));
#5838=DIRECTION('center_axis',(0.,0.,-1.));
#5839=DIRECTION('ref_axis',(1.,0.,0.));
#5840=DIRECTION('center_axis',(0.,0.,1.));
#5841=DIRECTION('ref_axis',(1.,0.,0.));
#5842=DIRECTION('center_axis',(0.,0.,1.));
#5843=DIRECTION('ref_axis',(1.,0.,0.));
#5844=DIRECTION('center_axis',(0.,0.,1.));
#5845=DIRECTION('ref_axis',(1.,0.,0.));
#5846=DIRECTION('',(0.,0.,1.));
#5847=DIRECTION('center_axis',(0.,0.,-1.));
#5848=DIRECTION('ref_axis',(1.,0.,0.));
#5849=DIRECTION('center_axis',(0.,0.,1.));
#5850=DIRECTION('ref_axis',(1.,0.,0.));
#5851=DIRECTION('center_axis',(1.,0.,0.));
#5852=DIRECTION('ref_axis',(0.,1.22464679914735E-16,1.));
#5853=DIRECTION('',(-1.,0.,0.));
#5854=DIRECTION('center_axis',(-1.,0.,0.));
#5855=DIRECTION('ref_axis',(0.,0.,-1.));
#5856=DIRECTION('',(1.,0.,0.));
#5857=DIRECTION('center_axis',(1.,0.,0.));
#5858=DIRECTION('ref_axis',(0.,0.,-1.));
#5859=DIRECTION('center_axis',(1.,0.,0.));
#5860=DIRECTION('ref_axis',(0.,1.,0.));
#5861=DIRECTION('',(0.,0.,1.));
#5862=DIRECTION('',(0.,1.,0.));
#5863=DIRECTION('',(0.,0.,1.));
#5864=DIRECTION('center_axis',(0.,1.,0.));
#5865=DIRECTION('ref_axis',(-1.,0.,0.));
#5866=DIRECTION('',(0.,0.,1.));
#5867=DIRECTION('',(-1.,0.,0.));
#5868=DIRECTION('center_axis',(0.,-1.,0.));
#5869=DIRECTION('ref_axis',(1.,0.,0.));
#5870=DIRECTION('',(1.,0.,0.));
#5871=DIRECTION('',(0.,0.,1.));
#5872=DIRECTION('center_axis',(-1.,0.,0.));
#5873=DIRECTION('ref_axis',(0.,-1.,0.));
#5874=DIRECTION('',(0.,-1.,0.));
#5875=DIRECTION('center_axis',(0.,0.,1.));
#5876=DIRECTION('ref_axis',(1.,0.,0.));
#5877=DIRECTION('axis',(0.,0.,1.));
#5878=DIRECTION('refdir',(1.,0.,0.));
#5879=DIRECTION('center_axis',(0.,0.,1.));
#5880=DIRECTION('ref_axis',(1.,0.,0.));
#5881=DIRECTION('center_axis',(0.,0.,-1.));
#5882=DIRECTION('ref_axis',(1.,0.,0.));
#5883=DIRECTION('',(0.,0.,-1.));
#5884=DIRECTION('center_axis',(0.,0.,-1.));
#5885=DIRECTION('ref_axis',(1.,0.,0.));
#5886=DIRECTION('center_axis',(0.,0.,1.));
#5887=DIRECTION('ref_axis',(1.,0.,0.));
#5888=DIRECTION('center_axis',(0.,0.,1.));
#5889=DIRECTION('ref_axis',(1.,0.,0.));
#5890=DIRECTION('axis',(0.,0.,1.));
#5891=DIRECTION('refdir',(1.,0.,0.));
#5892=DIRECTION('center_axis',(0.,0.,1.));
#5893=DIRECTION('ref_axis',(1.,0.,0.));
#5894=DIRECTION('center_axis',(0.,0.,-1.));
#5895=DIRECTION('ref_axis',(1.,0.,0.));
#5896=DIRECTION('',(0.,0.,-1.));
#5897=DIRECTION('center_axis',(0.,0.,-1.));
#5898=DIRECTION('ref_axis',(1.,0.,0.));
#5899=DIRECTION('center_axis',(0.,0.,1.));
#5900=DIRECTION('ref_axis',(1.,0.,0.));
#5901=DIRECTION('center_axis',(0.,0.,1.));
#5902=DIRECTION('ref_axis',(1.,0.,0.));
#5903=DIRECTION('axis',(0.,0.,1.));
#5904=DIRECTION('refdir',(1.,0.,0.));
#5905=DIRECTION('center_axis',(0.866025403784439,0.,-0.5));
#5906=DIRECTION('ref_axis',(0.5,0.,0.866025403784439));
#5907=DIRECTION('',(-0.5,0.,-0.866025403784439));
#5908=DIRECTION('',(0.,-1.,0.));
#5909=DIRECTION('',(0.5,0.,0.866025403784439));
#5910=DIRECTION('',(0.,-1.,0.));
#5911=DIRECTION('center_axis',(1.60246890531964E-16,0.,-1.));
#5912=DIRECTION('ref_axis',(1.,0.,1.60246890531964E-16));
#5913=DIRECTION('',(-1.,0.,-1.60246890531964E-16));
#5914=DIRECTION('',(0.,-1.,0.));
#5915=DIRECTION('',(1.,0.,1.60246890531964E-16));
#5916=DIRECTION('center_axis',(-0.866025403784439,0.,-0.5));
#5917=DIRECTION('ref_axis',(0.5,0.,-0.866025403784439));
#5918=DIRECTION('',(-0.5,0.,0.866025403784439));
#5919=DIRECTION('',(0.,-1.,0.));
#5920=DIRECTION('',(0.5,0.,-0.866025403784439));
#5921=DIRECTION('center_axis',(-0.866025403784439,0.,0.5));
#5922=DIRECTION('ref_axis',(-0.5,0.,-0.866025403784439));
#5923=DIRECTION('',(0.5,0.,0.866025403784439));
#5924=DIRECTION('',(0.,-1.,0.));
#5925=DIRECTION('',(-0.5,0.,-0.866025403784439));
#5926=DIRECTION('center_axis',(-1.60246890531964E-16,0.,1.));
#5927=DIRECTION('ref_axis',(-1.,0.,-1.60246890531964E-16));
#5928=DIRECTION('',(1.,0.,1.60246890531964E-16));
#5929=DIRECTION('',(0.,-1.,0.));
#5930=DIRECTION('',(-1.,0.,-1.60246890531964E-16));
#5931=DIRECTION('center_axis',(0.866025403784439,0.,0.5));
#5932=DIRECTION('ref_axis',(-0.5,0.,0.866025403784439));
#5933=DIRECTION('',(0.5,0.,-0.866025403784439));
#5934=DIRECTION('',(-0.5,0.,0.866025403784439));
#5935=DIRECTION('center_axis',(0.,1.,0.));
#5936=DIRECTION('ref_axis',(1.,0.,0.));
#5937=DIRECTION('center_axis',(0.,-1.,0.));
#5938=DIRECTION('ref_axis',(0.,0.,-1.));
#5939=DIRECTION('center_axis',(0.,1.,0.));
#5940=DIRECTION('ref_axis',(1.,0.,0.));
#5941=DIRECTION('center_axis',(0.,1.,0.));
#5942=DIRECTION('ref_axis',(1.,0.,0.));
#5943=DIRECTION('center_axis',(0.,1.,0.));
#5944=DIRECTION('ref_axis',(0.,0.,1.));
#5945=DIRECTION('center_axis',(0.,-1.,0.));
#5946=DIRECTION('ref_axis',(1.,0.,0.));
#5947=DIRECTION('center_axis',(0.,-1.,0.));
#5948=DIRECTION('ref_axis',(1.,0.,0.));
#5949=DIRECTION('center_axis',(0.,-1.,0.));
#5950=DIRECTION('ref_axis',(1.,0.,0.));
#5951=DIRECTION('',(0.707106781186547,0.707106781186548,8.65956056235493E-17));
#5952=DIRECTION('center_axis',(0.,-1.,0.));
#5953=DIRECTION('ref_axis',(1.,0.,0.));
#5954=DIRECTION('center_axis',(0.,-1.,0.));
#5955=DIRECTION('ref_axis',(1.,0.,0.));
#5956=DIRECTION('',(0.,1.,0.));
#5957=DIRECTION('center_axis',(0.,1.,0.));
#5958=DIRECTION('ref_axis',(1.,0.,0.));
#5959=DIRECTION('center_axis',(0.,-1.,0.));
#5960=DIRECTION('ref_axis',(1.,0.,0.));
#5961=DIRECTION('',(-0.707106781186547,0.707106781186548,-8.65956056235493E-17));
#5962=DIRECTION('center_axis',(0.,-1.,0.));
#5963=DIRECTION('ref_axis',(0.,0.,-1.));
#5964=DIRECTION('center_axis',(0.,-1.,0.));
#5965=DIRECTION('ref_axis',(1.,0.,0.));
#5966=DIRECTION('center_axis',(0.,1.,0.));
#5967=DIRECTION('ref_axis',(1.,0.,0.));
#5968=DIRECTION('center_axis',(0.,1.,0.));
#5969=DIRECTION('ref_axis',(1.,0.,0.));
#5970=DIRECTION('',(-0.447213595499958,0.894427190999916,-5.47678698264203E-17));
#5971=DIRECTION('center_axis',(0.,-1.,0.));
#5972=DIRECTION('ref_axis',(1.,0.,0.));
#5973=DIRECTION('',(0.,1.,0.));
#5974=DIRECTION('axis',(0.,0.,1.));
#5975=DIRECTION('refdir',(1.,0.,0.));
#5976=DIRECTION('center_axis',(0.,1.,0.));
#5977=DIRECTION('ref_axis',(1.,0.,0.));
#5978=DIRECTION('center_axis',(0.,-1.,0.));
#5979=DIRECTION('ref_axis',(1.,0.,0.));
#5980=DIRECTION('',(0.,-1.,0.));
#5981=DIRECTION('center_axis',(0.,-1.,0.));
#5982=DIRECTION('ref_axis',(1.,0.,0.));
#5983=DIRECTION('center_axis',(0.,1.,0.));
#5984=DIRECTION('ref_axis',(1.,0.,0.));
#5985=DIRECTION('center_axis',(0.,1.,0.));
#5986=DIRECTION('ref_axis',(1.,0.,0.));
#5987=DIRECTION('',(0.,-1.,0.));
#5988=DIRECTION('center_axis',(0.,1.,0.));
#5989=DIRECTION('ref_axis',(1.,0.,0.));
#5990=DIRECTION('center_axis',(0.,1.,0.));
#5991=DIRECTION('ref_axis',(1.,0.,0.));
#5992=DIRECTION('center_axis',(0.,1.,0.));
#5993=DIRECTION('ref_axis',(1.,0.,0.));
#5994=DIRECTION('axis',(0.,0.,1.));
#5995=DIRECTION('refdir',(1.,0.,0.));
#5996=DIRECTION('center_axis',(0.,1.,0.));
#5997=DIRECTION('ref_axis',(1.,0.,0.));
#5998=DIRECTION('',(0.866025403784439,-0.5,1.06057523872491E-16));
#5999=DIRECTION('center_axis',(0.,-1.,0.));
#6000=DIRECTION('ref_axis',(1.,0.,0.));
#6001=DIRECTION('center_axis',(0.,-1.,0.));
#6002=DIRECTION('ref_axis',(1.,0.,0.));
#6003=DIRECTION('center_axis',(0.,1.,0.));
#6004=DIRECTION('ref_axis',(1.,0.,0.));
#6005=DIRECTION('',(-0.866025403784439,-0.5,-1.06057523872491E-16));
#6006=DIRECTION('center_axis',(1.4792020664489E-16,0.,-1.));
#6007=DIRECTION('ref_axis',(-1.,0.,-1.4792020664489E-16));
#6008=DIRECTION('',(0.,1.,0.));
#6009=DIRECTION('',(0.,1.,0.));
#6010=DIRECTION('center_axis',(-0.866025403784439,0.,-0.5));
#6011=DIRECTION('ref_axis',(-0.5,0.,0.866025403784439));
#6012=DIRECTION('',(0.,1.,0.));
#6013=DIRECTION('center_axis',(-0.866025403784439,0.,0.5));
#6014=DIRECTION('ref_axis',(0.5,0.,0.866025403784439));
#6015=DIRECTION('',(0.,1.,0.));
#6016=DIRECTION('center_axis',(0.,1.,0.));
#6017=DIRECTION('ref_axis',(1.,0.,0.));
#6018=DIRECTION('center_axis',(0.,1.,0.));
#6019=DIRECTION('ref_axis',(1.,0.,0.));
#6020=DIRECTION('',(0.,-1.,0.));
#6021=DIRECTION('center_axis',(0.,1.,0.));
#6022=DIRECTION('ref_axis',(1.,0.,0.));
#6023=DIRECTION('center_axis',(-2.95840413289779E-16,0.,1.));
#6024=DIRECTION('ref_axis',(1.,0.,2.95840413289779E-16));
#6025=DIRECTION('',(0.,1.,0.));
#6026=DIRECTION('center_axis',(0.866025403784439,0.,-0.5));
#6027=DIRECTION('ref_axis',(-0.5,0.,-0.866025403784439));
#6028=DIRECTION('',(0.,1.,0.));
#6029=DIRECTION('center_axis',(0.866025403784439,0.,0.5));
#6030=DIRECTION('ref_axis',(0.5,0.,-0.866025403784439));
#6031=DIRECTION('center_axis',(0.,1.,0.));
#6032=DIRECTION('ref_axis',(1.,0.,0.));
#6033=DIRECTION('center_axis',(0.,1.,0.));
#6034=DIRECTION('ref_axis',(1.,0.,0.));
#6035=DIRECTION('',(0.,0.,1.));
#6036=DIRECTION('',(1.,0.,0.));
#6037=DIRECTION('',(0.,0.,1.));
#6038=DIRECTION('',(1.,0.,0.));
#6039=DIRECTION('',(0.,0.,1.));
#6040=DIRECTION('',(1.,0.,0.));
#6041=DIRECTION('',(0.,0.,1.));
#6042=DIRECTION('',(1.,0.,0.));
#6043=DIRECTION('',(0.,-1.,2.22044604925031E-16));
#6044=DIRECTION('',(1.,0.,0.));
#6045=DIRECTION('',(0.,-1.,2.22044604925031E-16));
#6046=DIRECTION('',(1.,0.,0.));
#6047=DIRECTION('',(0.,-1.,2.22044604925031E-16));
#6048=DIRECTION('',(1.,0.,0.));
#6049=DIRECTION('',(0.,-1.,2.22044604925031E-16));
#6050=DIRECTION('',(1.,0.,0.));
#6051=DIRECTION('',(0.,-1.,2.22044604925031E-16));
#6052=DIRECTION('',(1.,0.,0.));
#6053=DIRECTION('',(0.,-1.,2.22044604925031E-16));
#6054=DIRECTION('',(1.,0.,0.));
#6055=DIRECTION('',(0.,-1.,2.22044604925031E-16));
#6056=DIRECTION('',(1.,0.,0.));
#6057=DIRECTION('',(0.,-1.,2.22044604925031E-16));
#6058=DIRECTION('',(1.,0.,0.));
#6059=DIRECTION('',(0.,-1.,2.22044604925031E-16));
#6060=DIRECTION('',(1.,0.,0.));
#6061=DIRECTION('',(0.,-1.,2.22044604925031E-16));
#6062=DIRECTION('',(1.,0.,0.));
#6063=DIRECTION('axis',(0.,0.,1.));
#6064=DIRECTION('refdir',(1.,0.,0.));
#6065=DIRECTION('axis',(0.,0.,1.));
#6066=DIRECTION('refdir',(1.,0.,0.));
#6067=DIRECTION('center_axis',(1.,0.,0.));
#6068=DIRECTION('ref_axis',(0.,0.,-1.));
#6069=DIRECTION('center_axis',(1.,0.,0.));
#6070=DIRECTION('ref_axis',(0.,0.,-1.));
#6071=DIRECTION('',(-1.,0.,0.));
#6072=DIRECTION('center_axis',(1.,0.,0.));
#6073=DIRECTION('ref_axis',(0.,0.,-1.));
#6074=DIRECTION('center_axis',(1.,0.,0.));
#6075=DIRECTION('ref_axis',(0.,0.,-1.));
#6076=DIRECTION('center_axis',(1.,0.,0.));
#6077=DIRECTION('ref_axis',(0.,0.,-1.));
#6078=DIRECTION('',(0.,0.,1.));
#6079=DIRECTION('',(1.,0.,0.));
#6080=DIRECTION('',(0.,0.,1.));
#6081=DIRECTION('',(1.,0.,0.));
#6082=DIRECTION('',(0.,0.,1.));
#6083=DIRECTION('',(1.,0.,0.));
#6084=DIRECTION('',(0.,0.,1.));
#6085=DIRECTION('',(1.,0.,0.));
#6086=CARTESIAN_POINT('',(0.,0.,0.));
#6087=CARTESIAN_POINT('',(0.,0.,0.));
#6088=CARTESIAN_POINT('',(0.,0.,0.));
#6089=CARTESIAN_POINT('Origin',(12.5,-0.3,0.7));
#6090=CARTESIAN_POINT('',(14.5,-0.3,1.));
#6091=CARTESIAN_POINT('',(12.5,-0.3,1.));
#6092=CARTESIAN_POINT('',(11.25,-0.3,1.));
#6093=CARTESIAN_POINT('',(14.5,-0.3,0.7));
#6094=CARTESIAN_POINT('',(14.5,-0.3,0.7));
#6095=CARTESIAN_POINT('',(12.5,-0.3,0.7));
#6096=CARTESIAN_POINT('',(12.5,-0.3,0.7));
#6097=CARTESIAN_POINT('',(12.5,-0.3,0.7));
#6098=CARTESIAN_POINT('Origin',(12.5,0.3,0.7));
#6099=CARTESIAN_POINT('',(12.5,0.3,1.));
#6100=CARTESIAN_POINT('',(12.5,0.15,1.));
#6101=CARTESIAN_POINT('',(12.5,0.3,0.7));
#6102=CARTESIAN_POINT('',(12.5,0.3,0.7));
#6103=CARTESIAN_POINT('',(12.5,0.3,0.7));
#6104=CARTESIAN_POINT('Origin',(14.5,0.3,0.7));
#6105=CARTESIAN_POINT('',(14.5,0.3,1.));
#6106=CARTESIAN_POINT('',(12.25,0.3,1.));
#6107=CARTESIAN_POINT('',(14.5,0.3,0.7));
#6108=CARTESIAN_POINT('',(14.5,0.3,0.7));
#6109=CARTESIAN_POINT('',(14.5,0.3,0.7));
#6110=CARTESIAN_POINT('Origin',(14.5,-0.3,0.7));
#6111=CARTESIAN_POINT('',(14.5,-0.15,1.));
#6112=CARTESIAN_POINT('',(14.5,-0.3,0.7));
#6113=CARTESIAN_POINT('Origin',(13.5,0.,0.7));
#6114=CARTESIAN_POINT('Origin',(5.5,-0.3,0.7));
#6115=CARTESIAN_POINT('',(7.5,-0.3,1.));
#6116=CARTESIAN_POINT('',(5.5,-0.3,1.));
#6117=CARTESIAN_POINT('',(7.75,-0.3,1.));
#6118=CARTESIAN_POINT('',(7.5,-0.3,0.7));
#6119=CARTESIAN_POINT('',(7.5,-0.3,0.7));
#6120=CARTESIAN_POINT('',(5.5,-0.3,0.7));
#6121=CARTESIAN_POINT('',(5.5,-0.3,0.7));
#6122=CARTESIAN_POINT('',(5.5,-0.3,0.7));
#6123=CARTESIAN_POINT('Origin',(5.5,0.3,0.7));
#6124=CARTESIAN_POINT('',(5.5,0.3,1.));
#6125=CARTESIAN_POINT('',(5.5,0.15,1.));
#6126=CARTESIAN_POINT('',(5.5,0.3,0.7));
#6127=CARTESIAN_POINT('',(5.5,0.3,0.7));
#6128=CARTESIAN_POINT('',(5.5,0.3,0.7));
#6129=CARTESIAN_POINT('Origin',(7.5,0.3,0.7));
#6130=CARTESIAN_POINT('',(7.5,0.3,1.));
#6131=CARTESIAN_POINT('',(8.75,0.3,1.));
#6132=CARTESIAN_POINT('',(7.5,0.3,0.7));
#6133=CARTESIAN_POINT('',(7.5,0.3,0.7));
#6134=CARTESIAN_POINT('',(7.5,0.3,0.7));
#6135=CARTESIAN_POINT('Origin',(7.5,-0.3,0.7));
#6136=CARTESIAN_POINT('',(7.5,-0.15,1.));
#6137=CARTESIAN_POINT('',(7.5,-0.3,0.7));
#6138=CARTESIAN_POINT('Origin',(6.5,0.,0.7));
#6139=CARTESIAN_POINT('Origin',(17.,-4.5,-0.1));
#6140=CARTESIAN_POINT('',(16.725,-4.5,0.));
#6141=CARTESIAN_POINT('Origin',(17.,-4.5,0.));
#6142=CARTESIAN_POINT('',(16.725,-4.5,1.));
#6143=CARTESIAN_POINT('',(16.725,-4.5,-0.1));
#6144=CARTESIAN_POINT('Origin',(17.,-4.5,1.));
#6145=CARTESIAN_POINT('Origin',(3.,4.5,-0.1));
#6146=CARTESIAN_POINT('',(2.725,4.5,0.));
#6147=CARTESIAN_POINT('Origin',(3.,4.5,0.));
#6148=CARTESIAN_POINT('',(2.725,4.5,1.));
#6149=CARTESIAN_POINT('',(2.725,4.5,-0.1));
#6150=CARTESIAN_POINT('Origin',(3.,4.5,1.));
#6151=CARTESIAN_POINT('Origin',(3.,-4.5,-0.1));
#6152=CARTESIAN_POINT('',(2.725,-4.5,0.));
#6153=CARTESIAN_POINT('Origin',(3.,-4.5,0.));
#6154=CARTESIAN_POINT('',(2.725,-4.5,1.));
#6155=CARTESIAN_POINT('',(2.725,-4.5,-0.1));
#6156=CARTESIAN_POINT('Origin',(3.,-4.5,1.));
#6157=CARTESIAN_POINT('Origin',(17.,4.5,-0.1));
#6158=CARTESIAN_POINT('',(16.725,4.5,0.));
#6159=CARTESIAN_POINT('Origin',(17.,4.5,0.));
#6160=CARTESIAN_POINT('',(16.725,4.5,1.));
#6161=CARTESIAN_POINT('',(16.725,4.5,-0.1));
#6162=CARTESIAN_POINT('Origin',(17.,4.5,1.));
#6163=CARTESIAN_POINT('Origin',(10.,-4.,-0.1));
#6164=CARTESIAN_POINT('',(9.66,-4.,0.));
#6165=CARTESIAN_POINT('Origin',(10.,-4.,0.));
#6166=CARTESIAN_POINT('',(9.66,-4.,1.));
#6167=CARTESIAN_POINT('',(9.66,-4.,-0.1));
#6168=CARTESIAN_POINT('Origin',(10.,-4.,1.));
#6169=CARTESIAN_POINT('Origin',(10.,4.,-0.1));
#6170=CARTESIAN_POINT('',(9.66,4.,0.));
#6171=CARTESIAN_POINT('Origin',(10.,4.,0.));
#6172=CARTESIAN_POINT('',(9.66,4.,1.));
#6173=CARTESIAN_POINT('',(9.66,4.,-0.1));
#6174=CARTESIAN_POINT('Origin',(10.,4.,1.));
#6175=CARTESIAN_POINT('Origin',(2.,-1.4,-0.1));
#6176=CARTESIAN_POINT('',(1.75,-1.4,0.));
#6177=CARTESIAN_POINT('Origin',(2.,-1.4,0.));
#6178=CARTESIAN_POINT('',(1.75,-1.4,1.));
#6179=CARTESIAN_POINT('',(1.75,-1.4,-0.1));
#6180=CARTESIAN_POINT('Origin',(2.,-1.4,1.));
#6181=CARTESIAN_POINT('Origin',(6.5,-2.5,-0.1));
#6182=CARTESIAN_POINT('',(6.25,-2.5,0.));
#6183=CARTESIAN_POINT('Origin',(6.5,-2.5,0.));
#6184=CARTESIAN_POINT('',(6.25,-2.5,1.));
#6185=CARTESIAN_POINT('',(6.25,-2.5,-0.1));
#6186=CARTESIAN_POINT('Origin',(6.5,-2.5,1.));
#6187=CARTESIAN_POINT('Origin',(6.5,2.5,-0.1));
#6188=CARTESIAN_POINT('',(6.25,2.5,0.));
#6189=CARTESIAN_POINT('Origin',(6.5,2.5,0.));
#6190=CARTESIAN_POINT('',(6.25,2.5,1.));
#6191=CARTESIAN_POINT('',(6.25,2.5,-0.1));
#6192=CARTESIAN_POINT('Origin',(6.5,2.5,1.));
#6193=CARTESIAN_POINT('Origin',(13.5,-2.5,-0.1));
#6194=CARTESIAN_POINT('',(13.25,-2.5,0.));
#6195=CARTESIAN_POINT('Origin',(13.5,-2.5,0.));
#6196=CARTESIAN_POINT('',(13.25,-2.5,1.));
#6197=CARTESIAN_POINT('',(13.25,-2.5,-0.1));
#6198=CARTESIAN_POINT('Origin',(13.5,-2.5,1.));
#6199=CARTESIAN_POINT('Origin',(13.5,2.5,-0.1));
#6200=CARTESIAN_POINT('',(13.25,2.5,0.));
#6201=CARTESIAN_POINT('Origin',(13.5,2.5,0.));
#6202=CARTESIAN_POINT('',(13.25,2.5,1.));
#6203=CARTESIAN_POINT('',(13.25,2.5,-0.1));
#6204=CARTESIAN_POINT('Origin',(13.5,2.5,1.));
#6205=CARTESIAN_POINT('Origin',(2.,1.4,-0.1));
#6206=CARTESIAN_POINT('',(1.75,1.4,0.));
#6207=CARTESIAN_POINT('Origin',(2.,1.4,0.));
#6208=CARTESIAN_POINT('',(1.75,1.4,1.));
#6209=CARTESIAN_POINT('',(1.75,1.4,-0.1));
#6210=CARTESIAN_POINT('Origin',(2.,1.4,1.));
#6211=CARTESIAN_POINT('Origin',(20.,5.5,0.));
#6212=CARTESIAN_POINT('',(20.,5.5,0.));
#6213=CARTESIAN_POINT('',(0.,5.5,0.));
#6214=CARTESIAN_POINT('',(20.,5.5,0.));
#6215=CARTESIAN_POINT('',(0.,5.5,1.));
#6216=CARTESIAN_POINT('',(0.,5.5,0.));
#6217=CARTESIAN_POINT('',(20.,5.5,1.));
#6218=CARTESIAN_POINT('',(20.,5.5,1.));
#6219=CARTESIAN_POINT('',(20.,5.5,0.));
#6220=CARTESIAN_POINT('Origin',(20.,-5.5,0.));
#6221=CARTESIAN_POINT('',(20.,-5.5,0.));
#6222=CARTESIAN_POINT('',(20.,-5.5,0.));
#6223=CARTESIAN_POINT('',(20.,-5.5,1.));
#6224=CARTESIAN_POINT('',(20.,-5.5,1.));
#6225=CARTESIAN_POINT('',(20.,-5.5,0.));
#6226=CARTESIAN_POINT('Origin',(0.,-5.5,0.));
#6227=CARTESIAN_POINT('',(0.,-5.5,0.));
#6228=CARTESIAN_POINT('',(0.,-5.5,0.));
#6229=CARTESIAN_POINT('',(0.,-5.5,1.));
#6230=CARTESIAN_POINT('',(0.,-5.5,1.));
#6231=CARTESIAN_POINT('',(0.,-5.5,0.));
#6232=CARTESIAN_POINT('Origin',(0.,5.5,0.));
#6233=CARTESIAN_POINT('',(0.,5.5,0.));
#6234=CARTESIAN_POINT('',(0.,5.5,1.));
#6235=CARTESIAN_POINT('Origin',(10.,0.,1.));
#6236=CARTESIAN_POINT('Origin',(10.,0.,0.));
#6237=CARTESIAN_POINT('',(0.,0.,0.));
#6238=CARTESIAN_POINT('Origin',(3.,-4.5,-1.1));
#6239=CARTESIAN_POINT('',(2.79,-4.5,-1.));
#6240=CARTESIAN_POINT('Origin',(3.,-4.5,-1.));
#6241=CARTESIAN_POINT('',(2.79,-4.5,0.));
#6242=CARTESIAN_POINT('',(2.79,-4.5,-1.1));
#6243=CARTESIAN_POINT('Origin',(3.,-4.5,0.));
#6244=CARTESIAN_POINT('Origin',(3.,4.5,-1.1));
#6245=CARTESIAN_POINT('',(2.79,4.5,-1.));
#6246=CARTESIAN_POINT('Origin',(3.,4.5,-1.));
#6247=CARTESIAN_POINT('',(2.79,4.5,0.));
#6248=CARTESIAN_POINT('',(2.79,4.5,-1.1));
#6249=CARTESIAN_POINT('Origin',(3.,4.5,0.));
#6250=CARTESIAN_POINT('Origin',(4.,5.5,-1.));
#6251=CARTESIAN_POINT('',(4.,5.5,-1.));
#6252=CARTESIAN_POINT('',(2.,5.5,-1.));
#6253=CARTESIAN_POINT('',(4.,5.5,-1.));
#6254=CARTESIAN_POINT('',(2.,5.5,0.));
#6255=CARTESIAN_POINT('',(2.,5.5,-1.));
#6256=CARTESIAN_POINT('',(4.,5.5,0.));
#6257=CARTESIAN_POINT('',(4.,5.5,0.));
#6258=CARTESIAN_POINT('',(4.,5.5,-1.));
#6259=CARTESIAN_POINT('Origin',(4.,-5.5,-1.));
#6260=CARTESIAN_POINT('',(4.,-5.5,-1.));
#6261=CARTESIAN_POINT('',(4.,-5.5,-1.));
#6262=CARTESIAN_POINT('',(4.,-5.5,0.));
#6263=CARTESIAN_POINT('',(4.,-5.5,0.));
#6264=CARTESIAN_POINT('',(4.,-5.5,-1.));
#6265=CARTESIAN_POINT('Origin',(2.,-5.5,-1.));
#6266=CARTESIAN_POINT('',(2.,-5.5,-1.));
#6267=CARTESIAN_POINT('',(2.,-5.5,-1.));
#6268=CARTESIAN_POINT('',(2.,-5.5,0.));
#6269=CARTESIAN_POINT('',(2.,-5.5,0.));
#6270=CARTESIAN_POINT('',(2.,-5.5,-1.));
#6271=CARTESIAN_POINT('Origin',(2.,5.5,-1.));
#6272=CARTESIAN_POINT('',(2.,5.5,-1.));
#6273=CARTESIAN_POINT('',(2.,5.5,0.));
#6274=CARTESIAN_POINT('Origin',(3.,0.,0.));
#6275=CARTESIAN_POINT('Origin',(3.,0.,-1.));
#6276=CARTESIAN_POINT('',(0.,0.,0.));
#6277=CARTESIAN_POINT('Origin',(4.,5.5,-1.3));
#6278=CARTESIAN_POINT('',(4.,5.5,-1.3));
#6279=CARTESIAN_POINT('',(2.,5.5,-1.3));
#6280=CARTESIAN_POINT('',(4.,5.5,-1.3));
#6281=CARTESIAN_POINT('',(2.,5.5,-1.));
#6282=CARTESIAN_POINT('',(2.,5.5,-1.3));
#6283=CARTESIAN_POINT('',(4.,5.5,-1.));
#6284=CARTESIAN_POINT('',(4.,5.5,-1.));
#6285=CARTESIAN_POINT('',(4.,5.5,-1.3));
#6286=CARTESIAN_POINT('Origin',(4.,-5.5,-1.3));
#6287=CARTESIAN_POINT('',(4.,-5.5,-1.3));
#6288=CARTESIAN_POINT('',(4.,-5.5,-1.3));
#6289=CARTESIAN_POINT('',(4.,-5.5,-1.));
#6290=CARTESIAN_POINT('',(4.,-5.5,-1.));
#6291=CARTESIAN_POINT('',(4.,-5.5,-1.3));
#6292=CARTESIAN_POINT('Origin',(2.,-5.5,-1.3));
#6293=CARTESIAN_POINT('',(2.,-5.5,-1.3));
#6294=CARTESIAN_POINT('',(2.,-5.5,-1.3));
#6295=CARTESIAN_POINT('',(2.,-5.5,-1.));
#6296=CARTESIAN_POINT('',(2.,-5.5,-1.));
#6297=CARTESIAN_POINT('',(2.,-5.5,-1.3));
#6298=CARTESIAN_POINT('Origin',(2.,5.5,-1.3));
#6299=CARTESIAN_POINT('',(2.,5.5,-1.3));
#6300=CARTESIAN_POINT('',(2.,5.5,-1.));
#6301=CARTESIAN_POINT('Origin',(3.,0.,-1.));
#6302=CARTESIAN_POINT('Origin',(3.,0.,-1.3));
#6303=CARTESIAN_POINT('',(0.,0.,0.));
#6304=CARTESIAN_POINT('Origin',(17.,-4.5,-1.1));
#6305=CARTESIAN_POINT('',(16.79,-4.5,-1.));
#6306=CARTESIAN_POINT('Origin',(17.,-4.5,-1.));
#6307=CARTESIAN_POINT('',(16.79,-4.5,0.));
#6308=CARTESIAN_POINT('',(16.79,-4.5,-1.1));
#6309=CARTESIAN_POINT('Origin',(17.,-4.5,0.));
#6310=CARTESIAN_POINT('Origin',(17.,4.5,-1.1));
#6311=CARTESIAN_POINT('',(16.79,4.5,-1.));
#6312=CARTESIAN_POINT('Origin',(17.,4.5,-1.));
#6313=CARTESIAN_POINT('',(16.79,4.5,0.));
#6314=CARTESIAN_POINT('',(16.79,4.5,-1.1));
#6315=CARTESIAN_POINT('Origin',(17.,4.5,0.));
#6316=CARTESIAN_POINT('Origin',(18.,5.5,-1.));
#6317=CARTESIAN_POINT('',(18.,5.5,-1.));
#6318=CARTESIAN_POINT('',(16.,5.5,-1.));
#6319=CARTESIAN_POINT('',(18.,5.5,-1.));
#6320=CARTESIAN_POINT('',(16.,5.5,0.));
#6321=CARTESIAN_POINT('',(16.,5.5,-1.));
#6322=CARTESIAN_POINT('',(18.,5.5,0.));
#6323=CARTESIAN_POINT('',(18.,5.5,0.));
#6324=CARTESIAN_POINT('',(18.,5.5,-1.));
#6325=CARTESIAN_POINT('Origin',(18.,-5.5,-1.));
#6326=CARTESIAN_POINT('',(18.,-5.5,-1.));
#6327=CARTESIAN_POINT('',(18.,-5.5,-1.));
#6328=CARTESIAN_POINT('',(18.,-5.5,0.));
#6329=CARTESIAN_POINT('',(18.,-5.5,0.));
#6330=CARTESIAN_POINT('',(18.,-5.5,-1.));
#6331=CARTESIAN_POINT('Origin',(16.,-5.5,-1.));
#6332=CARTESIAN_POINT('',(16.,-5.5,-1.));
#6333=CARTESIAN_POINT('',(16.,-5.5,-1.));
#6334=CARTESIAN_POINT('',(16.,-5.5,0.));
#6335=CARTESIAN_POINT('',(16.,-5.5,0.));
#6336=CARTESIAN_POINT('',(16.,-5.5,-1.));
#6337=CARTESIAN_POINT('Origin',(16.,5.5,-1.));
#6338=CARTESIAN_POINT('',(16.,5.5,-1.));
#6339=CARTESIAN_POINT('',(16.,5.5,0.));
#6340=CARTESIAN_POINT('Origin',(17.,0.,0.));
#6341=CARTESIAN_POINT('Origin',(17.,0.,-1.));
#6342=CARTESIAN_POINT('',(0.,0.,0.));
#6343=CARTESIAN_POINT('Origin',(18.,5.5,-1.3));
#6344=CARTESIAN_POINT('',(18.,5.5,-1.3));
#6345=CARTESIAN_POINT('',(16.,5.5,-1.3));
#6346=CARTESIAN_POINT('',(18.,5.5,-1.3));
#6347=CARTESIAN_POINT('',(16.,5.5,-1.));
#6348=CARTESIAN_POINT('',(16.,5.5,-1.3));
#6349=CARTESIAN_POINT('',(18.,5.5,-1.));
#6350=CARTESIAN_POINT('',(18.,5.5,-1.));
#6351=CARTESIAN_POINT('',(18.,5.5,-1.3));
#6352=CARTESIAN_POINT('Origin',(18.,-5.5,-1.3));
#6353=CARTESIAN_POINT('',(18.,-5.5,-1.3));
#6354=CARTESIAN_POINT('',(18.,-5.5,-1.3));
#6355=CARTESIAN_POINT('',(18.,-5.5,-1.));
#6356=CARTESIAN_POINT('',(18.,-5.5,-1.));
#6357=CARTESIAN_POINT('',(18.,-5.5,-1.3));
#6358=CARTESIAN_POINT('Origin',(16.,-5.5,-1.3));
#6359=CARTESIAN_POINT('',(16.,-5.5,-1.3));
#6360=CARTESIAN_POINT('',(16.,-5.5,-1.3));
#6361=CARTESIAN_POINT('',(16.,-5.5,-1.));
#6362=CARTESIAN_POINT('',(16.,-5.5,-1.));
#6363=CARTESIAN_POINT('',(16.,-5.5,-1.3));
#6364=CARTESIAN_POINT('Origin',(16.,5.5,-1.3));
#6365=CARTESIAN_POINT('',(16.,5.5,-1.3));
#6366=CARTESIAN_POINT('',(16.,5.5,-1.));
#6367=CARTESIAN_POINT('Origin',(17.,0.,-1.));
#6368=CARTESIAN_POINT('Origin',(17.,0.,-1.3));
#6369=CARTESIAN_POINT('',(0.,0.,0.));
#6370=CARTESIAN_POINT('Origin',(6.5,2.5,2.5));
#6371=CARTESIAN_POINT('',(6.,2.5,2.5));
#6372=CARTESIAN_POINT('',(6.,2.5,5.));
#6373=CARTESIAN_POINT('',(6.,2.5,2.5));
#6374=CARTESIAN_POINT('',(6.5,3.,2.5));
#6375=CARTESIAN_POINT('Origin',(6.5,2.5,2.5));
#6376=CARTESIAN_POINT('',(6.5,3.,5.));
#6377=CARTESIAN_POINT('',(6.5,3.,2.5));
#6378=CARTESIAN_POINT('Origin',(6.5,2.5,5.));
#6379=CARTESIAN_POINT('Origin',(6.5,-2.5,2.5));
#6380=CARTESIAN_POINT('',(6.,-2.5,2.5));
#6381=CARTESIAN_POINT('',(6.,-2.5,5.));
#6382=CARTESIAN_POINT('',(6.,-2.5,2.5));
#6383=CARTESIAN_POINT('',(6.5,-3.,2.5));
#6384=CARTESIAN_POINT('Origin',(6.5,-2.5,2.5));
#6385=CARTESIAN_POINT('',(6.5,-3.,5.));
#6386=CARTESIAN_POINT('',(6.5,-3.,2.5));
#6387=CARTESIAN_POINT('',(7.,-2.5,5.));
#6388=CARTESIAN_POINT('Origin',(6.5,-2.5,5.));
#6389=CARTESIAN_POINT('Origin',(6.5,-2.5,5.));
#6390=CARTESIAN_POINT('Origin',(5.5,-0.3,0.9));
#6391=CARTESIAN_POINT('',(5.5,-0.3,1.));
#6392=CARTESIAN_POINT('',(7.5,-0.3,1.));
#6393=CARTESIAN_POINT('',(6.,-0.3,1.));
#6394=CARTESIAN_POINT('',(5.5,-0.3,1.3));
#6395=CARTESIAN_POINT('',(5.5,-0.3,0.9));
#6396=CARTESIAN_POINT('',(7.5,-0.3,1.3));
#6397=CARTESIAN_POINT('',(5.5,-0.3,1.3));
#6398=CARTESIAN_POINT('',(7.5,-0.3,0.9));
#6399=CARTESIAN_POINT('Origin',(7.5,-0.3,0.9));
#6400=CARTESIAN_POINT('',(7.5,0.3,1.));
#6401=CARTESIAN_POINT('',(7.5,-0.15,1.));
#6402=CARTESIAN_POINT('',(7.5,0.3,1.3));
#6403=CARTESIAN_POINT('',(7.5,-0.3,1.3));
#6404=CARTESIAN_POINT('',(7.5,0.3,0.9));
#6405=CARTESIAN_POINT('Origin',(7.5,0.3,0.9));
#6406=CARTESIAN_POINT('',(5.5,0.3,1.));
#6407=CARTESIAN_POINT('',(7.,0.3,1.));
#6408=CARTESIAN_POINT('',(5.5,0.3,1.3));
#6409=CARTESIAN_POINT('',(7.5,0.3,1.3));
#6410=CARTESIAN_POINT('',(5.5,0.3,0.9));
#6411=CARTESIAN_POINT('Origin',(5.5,0.3,0.9));
#6412=CARTESIAN_POINT('',(5.5,0.15,1.));
#6413=CARTESIAN_POINT('',(5.5,0.3,1.3));
#6414=CARTESIAN_POINT('Origin',(6.5,0.,1.3));
#6415=CARTESIAN_POINT('Origin',(6.5,-2.5,2.5));
#6416=CARTESIAN_POINT('Origin',(6.5,-2.5,5.));
#6417=CARTESIAN_POINT('',(6.5,-3.,2.5));
#6418=CARTESIAN_POINT('Origin',(6.5,-2.5,2.5));
#6419=CARTESIAN_POINT('Origin',(6.5,-2.5,2.5));
#6420=CARTESIAN_POINT('',(6.17,-2.5,2.5));
#6421=CARTESIAN_POINT('Origin',(6.5,-2.5,2.5));
#6422=CARTESIAN_POINT('Origin',(6.5,2.5,2.5));
#6423=CARTESIAN_POINT('',(7.,2.5,5.));
#6424=CARTESIAN_POINT('Origin',(6.5,2.5,5.));
#6425=CARTESIAN_POINT('Origin',(6.5,2.5,5.));
#6426=CARTESIAN_POINT('',(6.5,3.,2.5));
#6427=CARTESIAN_POINT('Origin',(6.5,2.5,2.5));
#6428=CARTESIAN_POINT('Origin',(6.5,2.5,2.5));
#6429=CARTESIAN_POINT('',(6.17,2.5,2.5));
#6430=CARTESIAN_POINT('Origin',(6.5,2.5,2.5));
#6431=CARTESIAN_POINT('Origin',(4.9,-2.6,5.1));
#6432=CARTESIAN_POINT('',(8.,-2.5,5.));
#6433=CARTESIAN_POINT('',(5.7,-2.5,5.));
#6434=CARTESIAN_POINT('',(8.,0.,2.5));
#6435=CARTESIAN_POINT('',(8.,-1.675,4.175));
#6436=CARTESIAN_POINT('',(5.,0.,2.5));
#6437=CARTESIAN_POINT('',(4.9,0.,2.5));
#6438=CARTESIAN_POINT('',(5.,-2.5,5.));
#6439=CARTESIAN_POINT('',(5.,-0.175,2.675));
#6440=CARTESIAN_POINT('',(5.7,-2.5,5.));
#6441=CARTESIAN_POINT('Origin',(6.5,0.,5.));
#6442=CARTESIAN_POINT('',(8.,-3.,5.));
#6443=CARTESIAN_POINT('',(5.,-3.,5.));
#6444=CARTESIAN_POINT('',(8.,-3.,5.));
#6445=CARTESIAN_POINT('Origin',(4.9,0.,2.5));
#6446=CARTESIAN_POINT('',(5.,2.5,5.));
#6447=CARTESIAN_POINT('',(5.7,2.5,5.));
#6448=CARTESIAN_POINT('',(5.,0.375,2.875));
#6449=CARTESIAN_POINT('',(8.,2.5,5.));
#6450=CARTESIAN_POINT('',(8.,-1.125,1.375));
#6451=CARTESIAN_POINT('',(5.7,2.5,5.));
#6452=CARTESIAN_POINT('Origin',(6.5,0.,5.));
#6453=CARTESIAN_POINT('',(5.,3.,5.));
#6454=CARTESIAN_POINT('',(8.,3.,5.));
#6455=CARTESIAN_POINT('',(5.,3.,5.));
#6456=CARTESIAN_POINT('Origin',(6.5,-2.5,0.9));
#6457=CARTESIAN_POINT('',(6.17,-2.5,1.));
#6458=CARTESIAN_POINT('Origin',(6.5,-2.5,1.));
#6459=CARTESIAN_POINT('',(6.17,-2.5,0.9));
#6460=CARTESIAN_POINT('Origin',(6.5,2.5,0.9));
#6461=CARTESIAN_POINT('',(6.17,2.5,1.));
#6462=CARTESIAN_POINT('Origin',(6.5,2.5,1.));
#6463=CARTESIAN_POINT('',(6.17,2.5,0.9));
#6464=CARTESIAN_POINT('Origin',(6.5,0.,5.));
#6465=CARTESIAN_POINT('',(5.,-3.,5.));
#6466=CARTESIAN_POINT('',(5.,3.,5.));
#6467=CARTESIAN_POINT('',(5.,-3.,5.));
#6468=CARTESIAN_POINT('Origin',(6.5,0.,5.));
#6469=CARTESIAN_POINT('',(8.,3.,5.));
#6470=CARTESIAN_POINT('',(8.,-3.,5.));
#6471=CARTESIAN_POINT('',(8.,3.,5.));
#6472=CARTESIAN_POINT('Origin',(5.,3.,1.));
#6473=CARTESIAN_POINT('',(5.,3.,1.));
#6474=CARTESIAN_POINT('',(5.,3.,1.));
#6475=CARTESIAN_POINT('',(5.,-3.,1.));
#6476=CARTESIAN_POINT('',(5.,3.,1.));
#6477=CARTESIAN_POINT('',(5.,-3.,1.));
#6478=CARTESIAN_POINT('Origin',(8.,3.,1.));
#6479=CARTESIAN_POINT('',(8.,3.,1.));
#6480=CARTESIAN_POINT('',(8.,3.,1.));
#6481=CARTESIAN_POINT('',(8.,3.,1.));
#6482=CARTESIAN_POINT('Origin',(8.,-3.,1.));
#6483=CARTESIAN_POINT('',(8.,-3.,1.));
#6484=CARTESIAN_POINT('',(8.,-3.,1.));
#6485=CARTESIAN_POINT('',(8.,-3.,1.));
#6486=CARTESIAN_POINT('Origin',(5.,-3.,1.));
#6487=CARTESIAN_POINT('',(5.,-3.,1.));
#6488=CARTESIAN_POINT('Origin',(6.5,0.,1.));
#6489=CARTESIAN_POINT('',(0.,0.,0.));
#6490=CARTESIAN_POINT('Origin',(13.5,2.5,2.5));
#6491=CARTESIAN_POINT('',(13.,2.5,2.5));
#6492=CARTESIAN_POINT('',(13.,2.5,5.));
#6493=CARTESIAN_POINT('',(13.,2.5,2.5));
#6494=CARTESIAN_POINT('',(13.5,3.,2.5));
#6495=CARTESIAN_POINT('Origin',(13.5,2.5,2.5));
#6496=CARTESIAN_POINT('',(13.5,3.,5.));
#6497=CARTESIAN_POINT('',(13.5,3.,2.5));
#6498=CARTESIAN_POINT('Origin',(13.5,2.5,5.));
#6499=CARTESIAN_POINT('Origin',(13.5,-2.5,2.5));
#6500=CARTESIAN_POINT('',(13.,-2.5,2.5));
#6501=CARTESIAN_POINT('',(13.,-2.5,5.));
#6502=CARTESIAN_POINT('',(13.,-2.5,2.5));
#6503=CARTESIAN_POINT('',(13.5,-3.,2.5));
#6504=CARTESIAN_POINT('Origin',(13.5,-2.5,2.5));
#6505=CARTESIAN_POINT('',(13.5,-3.,5.));
#6506=CARTESIAN_POINT('',(13.5,-3.,2.5));
#6507=CARTESIAN_POINT('',(14.,-2.5,5.));
#6508=CARTESIAN_POINT('Origin',(13.5,-2.5,5.));
#6509=CARTESIAN_POINT('Origin',(13.5,-2.5,5.));
#6510=CARTESIAN_POINT('Origin',(12.5,-0.3,0.9));
#6511=CARTESIAN_POINT('',(12.5,-0.3,1.));
#6512=CARTESIAN_POINT('',(14.5,-0.3,1.));
#6513=CARTESIAN_POINT('',(13.,-0.3,1.));
#6514=CARTESIAN_POINT('',(12.5,-0.3,1.3));
#6515=CARTESIAN_POINT('',(12.5,-0.3,0.9));
#6516=CARTESIAN_POINT('',(14.5,-0.3,1.3));
#6517=CARTESIAN_POINT('',(12.5,-0.3,1.3));
#6518=CARTESIAN_POINT('',(14.5,-0.3,0.9));
#6519=CARTESIAN_POINT('Origin',(14.5,-0.3,0.9));
#6520=CARTESIAN_POINT('',(14.5,0.3,1.));
#6521=CARTESIAN_POINT('',(14.5,-0.15,1.));
#6522=CARTESIAN_POINT('',(14.5,0.3,1.3));
#6523=CARTESIAN_POINT('',(14.5,-0.3,1.3));
#6524=CARTESIAN_POINT('',(14.5,0.3,0.9));
#6525=CARTESIAN_POINT('Origin',(14.5,0.3,0.9));
#6526=CARTESIAN_POINT('',(12.5,0.3,1.));
#6527=CARTESIAN_POINT('',(14.,0.3,1.));
#6528=CARTESIAN_POINT('',(12.5,0.3,1.3));
#6529=CARTESIAN_POINT('',(14.5,0.3,1.3));
#6530=CARTESIAN_POINT('',(12.5,0.3,0.9));
#6531=CARTESIAN_POINT('Origin',(12.5,0.3,0.9));
#6532=CARTESIAN_POINT('',(12.5,0.15,1.));
#6533=CARTESIAN_POINT('',(12.5,0.3,1.3));
#6534=CARTESIAN_POINT('Origin',(13.5,0.,1.3));
#6535=CARTESIAN_POINT('Origin',(13.5,-2.5,2.5));
#6536=CARTESIAN_POINT('Origin',(13.5,-2.5,5.));
#6537=CARTESIAN_POINT('',(13.5,-3.,2.5));
#6538=CARTESIAN_POINT('Origin',(13.5,-2.5,2.5));
#6539=CARTESIAN_POINT('Origin',(13.5,-2.5,2.5));
#6540=CARTESIAN_POINT('',(13.17,-2.5,2.5));
#6541=CARTESIAN_POINT('Origin',(13.5,-2.5,2.5));
#6542=CARTESIAN_POINT('Origin',(13.5,2.5,2.5));
#6543=CARTESIAN_POINT('',(14.,2.5,5.));
#6544=CARTESIAN_POINT('Origin',(13.5,2.5,5.));
#6545=CARTESIAN_POINT('Origin',(13.5,2.5,5.));
#6546=CARTESIAN_POINT('',(13.5,3.,2.5));
#6547=CARTESIAN_POINT('Origin',(13.5,2.5,2.5));
#6548=CARTESIAN_POINT('Origin',(13.5,2.5,2.5));
#6549=CARTESIAN_POINT('',(13.17,2.5,2.5));
#6550=CARTESIAN_POINT('Origin',(13.5,2.5,2.5));
#6551=CARTESIAN_POINT('Origin',(11.9,-2.6,5.1));
#6552=CARTESIAN_POINT('',(15.,-2.5,5.));
#6553=CARTESIAN_POINT('',(12.7,-2.5,5.));
#6554=CARTESIAN_POINT('',(15.,0.,2.5));
#6555=CARTESIAN_POINT('',(15.,-1.675,4.175));
#6556=CARTESIAN_POINT('',(12.,0.,2.5));
#6557=CARTESIAN_POINT('',(11.9,0.,2.5));
#6558=CARTESIAN_POINT('',(12.,-2.5,5.));
#6559=CARTESIAN_POINT('',(12.,-0.175,2.675));
#6560=CARTESIAN_POINT('',(12.7,-2.5,5.));
#6561=CARTESIAN_POINT('Origin',(13.5,0.,5.));
#6562=CARTESIAN_POINT('',(15.,-3.,5.));
#6563=CARTESIAN_POINT('',(12.,-3.,5.));
#6564=CARTESIAN_POINT('',(15.,-3.,5.));
#6565=CARTESIAN_POINT('Origin',(11.9,0.,2.5));
#6566=CARTESIAN_POINT('',(12.,2.5,5.));
#6567=CARTESIAN_POINT('',(12.7,2.5,5.));
#6568=CARTESIAN_POINT('',(12.,0.375,2.875));
#6569=CARTESIAN_POINT('',(15.,2.5,5.));
#6570=CARTESIAN_POINT('',(15.,-1.125,1.375));
#6571=CARTESIAN_POINT('',(12.7,2.5,5.));
#6572=CARTESIAN_POINT('Origin',(13.5,0.,5.));
#6573=CARTESIAN_POINT('',(12.,3.,5.));
#6574=CARTESIAN_POINT('',(15.,3.,5.));
#6575=CARTESIAN_POINT('',(12.,3.,5.));
#6576=CARTESIAN_POINT('Origin',(13.5,-2.5,0.9));
#6577=CARTESIAN_POINT('',(13.17,-2.5,1.));
#6578=CARTESIAN_POINT('Origin',(13.5,-2.5,1.));
#6579=CARTESIAN_POINT('',(13.17,-2.5,0.9));
#6580=CARTESIAN_POINT('Origin',(13.5,2.5,0.9));
#6581=CARTESIAN_POINT('',(13.17,2.5,1.));
#6582=CARTESIAN_POINT('Origin',(13.5,2.5,1.));
#6583=CARTESIAN_POINT('',(13.17,2.5,0.9));
#6584=CARTESIAN_POINT('Origin',(13.5,0.,5.));
#6585=CARTESIAN_POINT('',(12.,-3.,5.));
#6586=CARTESIAN_POINT('',(12.,3.,5.));
#6587=CARTESIAN_POINT('',(12.,-3.,5.));
#6588=CARTESIAN_POINT('Origin',(13.5,0.,5.));
#6589=CARTESIAN_POINT('',(15.,3.,5.));
#6590=CARTESIAN_POINT('',(15.,-3.,5.));
#6591=CARTESIAN_POINT('',(15.,3.,5.));
#6592=CARTESIAN_POINT('Origin',(12.,3.,1.));
#6593=CARTESIAN_POINT('',(12.,3.,1.));
#6594=CARTESIAN_POINT('',(12.,3.,1.));
#6595=CARTESIAN_POINT('',(12.,-3.,1.));
#6596=CARTESIAN_POINT('',(12.,3.,1.));
#6597=CARTESIAN_POINT('',(12.,-3.,1.));
#6598=CARTESIAN_POINT('Origin',(15.,3.,1.));
#6599=CARTESIAN_POINT('',(15.,3.,1.));
#6600=CARTESIAN_POINT('',(15.,3.,1.));
#6601=CARTESIAN_POINT('',(15.,3.,1.));
#6602=CARTESIAN_POINT('Origin',(15.,-3.,1.));
#6603=CARTESIAN_POINT('',(15.,-3.,1.));
#6604=CARTESIAN_POINT('',(15.,-3.,1.));
#6605=CARTESIAN_POINT('',(15.,-3.,1.));
#6606=CARTESIAN_POINT('Origin',(12.,-3.,1.));
#6607=CARTESIAN_POINT('',(12.,-3.,1.));
#6608=CARTESIAN_POINT('Origin',(13.5,0.,1.));
#6609=CARTESIAN_POINT('',(0.,0.,0.));
#6610=CARTESIAN_POINT('Origin',(1.4,0.,4.62132034355964));
#6611=CARTESIAN_POINT('',(1.5,-2.57175827820944E-17,4.83132034355964));
#6612=CARTESIAN_POINT('Origin',(1.5,0.,4.62132034355964));
#6613=CARTESIAN_POINT('',(2.5,2.57175827820944E-17,4.83132034355964));
#6614=CARTESIAN_POINT('',(1.4,-2.57175827820944E-17,4.83132034355964));
#6615=CARTESIAN_POINT('Origin',(2.5,0.,4.62132034355964));
#6616=CARTESIAN_POINT('Origin',(2.,-1.4,2.5));
#6617=CARTESIAN_POINT('',(2.5,-1.4,2.5));
#6618=CARTESIAN_POINT('',(2.5,-1.4,5.5));
#6619=CARTESIAN_POINT('',(2.5,-1.4,2.5));
#6620=CARTESIAN_POINT('',(1.5,-1.4,5.5));
#6621=CARTESIAN_POINT('Origin',(2.,-1.4,5.5));
#6622=CARTESIAN_POINT('',(1.5,-1.4,2.5));
#6623=CARTESIAN_POINT('',(1.5,-1.4,2.5));
#6624=CARTESIAN_POINT('Origin',(2.,-1.4,2.5));
#6625=CARTESIAN_POINT('Origin',(2.,-1.4,2.5));
#6626=CARTESIAN_POINT('',(2.5,-1.4,2.5));
#6627=CARTESIAN_POINT('Origin',(2.,-1.4,2.5));
#6628=CARTESIAN_POINT('',(1.5,-1.4,2.5));
#6629=CARTESIAN_POINT('Origin',(2.,-1.4,5.5));
#6630=CARTESIAN_POINT('Origin',(2.,-1.4,2.5));
#6631=CARTESIAN_POINT('',(1.67,-1.4,2.5));
#6632=CARTESIAN_POINT('Origin',(2.,-1.4,2.5));
#6633=CARTESIAN_POINT('Origin',(2.,1.4,2.5));
#6634=CARTESIAN_POINT('',(2.5,1.4,2.5));
#6635=CARTESIAN_POINT('',(2.5,1.4,5.5));
#6636=CARTESIAN_POINT('',(2.5,1.4,2.5));
#6637=CARTESIAN_POINT('',(1.5,1.4,5.5));
#6638=CARTESIAN_POINT('Origin',(2.,1.4,5.5));
#6639=CARTESIAN_POINT('',(1.5,1.4,2.5));
#6640=CARTESIAN_POINT('',(1.5,1.4,2.5));
#6641=CARTESIAN_POINT('Origin',(2.,1.4,2.5));
#6642=CARTESIAN_POINT('Origin',(2.,1.4,2.5));
#6643=CARTESIAN_POINT('',(2.5,1.4,2.5));
#6644=CARTESIAN_POINT('Origin',(2.,1.4,2.5));
#6645=CARTESIAN_POINT('',(1.5,1.4,2.5));
#6646=CARTESIAN_POINT('Origin',(2.,1.4,5.5));
#6647=CARTESIAN_POINT('Origin',(2.,1.4,2.5));
#6648=CARTESIAN_POINT('',(1.67,1.4,2.5));
#6649=CARTESIAN_POINT('Origin',(2.,1.4,2.5));
#6650=CARTESIAN_POINT('Origin',(2.,0.,5.5));
#6651=CARTESIAN_POINT('',(2.5,2.,5.5));
#6652=CARTESIAN_POINT('',(2.5,-2.,5.5));
#6653=CARTESIAN_POINT('',(1.5,2.,5.5));
#6654=CARTESIAN_POINT('',(2.5,2.,5.5));
#6655=CARTESIAN_POINT('',(1.5,2.,5.5));
#6656=CARTESIAN_POINT('Origin',(2.,0.,5.5));
#6657=CARTESIAN_POINT('',(2.5,-2.,5.5));
#6658=CARTESIAN_POINT('',(1.5,2.,5.5));
#6659=CARTESIAN_POINT('Origin',(2.,0.,5.5));
#6660=CARTESIAN_POINT('',(1.5,-2.,5.5));
#6661=CARTESIAN_POINT('',(1.5,2.,5.5));
#6662=CARTESIAN_POINT('',(2.5,-2.,5.5));
#6663=CARTESIAN_POINT('',(1.5,-2.,5.5));
#6664=CARTESIAN_POINT('',(2.5,-2.,5.5));
#6665=CARTESIAN_POINT('Origin',(2.,-1.4,0.9));
#6666=CARTESIAN_POINT('',(1.67,-1.4,1.));
#6667=CARTESIAN_POINT('Origin',(2.,-1.4,1.));
#6668=CARTESIAN_POINT('',(1.67,-1.4,0.9));
#6669=CARTESIAN_POINT('Origin',(2.,1.4,0.9));
#6670=CARTESIAN_POINT('',(1.67,1.4,1.));
#6671=CARTESIAN_POINT('Origin',(2.,1.4,1.));
#6672=CARTESIAN_POINT('',(1.67,1.4,0.9));
#6673=CARTESIAN_POINT('Origin',(2.5,2.,1.));
#6674=CARTESIAN_POINT('',(2.5,2.,1.));
#6675=CARTESIAN_POINT('',(1.5,2.,1.));
#6676=CARTESIAN_POINT('',(2.5,2.,1.));
#6677=CARTESIAN_POINT('',(1.5,2.,1.));
#6678=CARTESIAN_POINT('',(2.5,2.,1.));
#6679=CARTESIAN_POINT('Origin',(2.5,-2.,1.));
#6680=CARTESIAN_POINT('',(2.5,-2.,1.));
#6681=CARTESIAN_POINT('',(2.5,-2.,1.));
#6682=CARTESIAN_POINT('',(2.5,-2.,1.));
#6683=CARTESIAN_POINT('Origin',(1.5,-2.,1.));
#6684=CARTESIAN_POINT('',(1.5,-2.,1.));
#6685=CARTESIAN_POINT('',(1.5,-2.,1.));
#6686=CARTESIAN_POINT('',(1.5,-2.,1.));
#6687=CARTESIAN_POINT('Origin',(1.5,2.,1.));
#6688=CARTESIAN_POINT('',(1.5,2.,1.));
#6689=CARTESIAN_POINT('Origin',(2.,0.,1.));
#6690=CARTESIAN_POINT('',(0.,0.,0.));
#6691=CARTESIAN_POINT('Origin',(-1.,0.,0.35));
#6692=CARTESIAN_POINT('',(-1.,-0.26,0.6));
#6693=CARTESIAN_POINT('',(-1.,-0.3,0.56));
#6694=CARTESIAN_POINT('',(-1.,-0.2675,0.5925));
#6695=CARTESIAN_POINT('',(-1.,0.26,0.6));
#6696=CARTESIAN_POINT('',(-1.,0.,0.6));
#6697=CARTESIAN_POINT('',(-1.,0.3,0.56));
#6698=CARTESIAN_POINT('',(-1.,0.2675,0.5925));
#6699=CARTESIAN_POINT('',(-1.,0.3,0.04));
#6700=CARTESIAN_POINT('',(-1.,0.3,0.175));
#6701=CARTESIAN_POINT('',(-1.,0.26,0.));
#6702=CARTESIAN_POINT('',(-1.,0.2925,0.0325));
#6703=CARTESIAN_POINT('',(-1.,-0.26,0.));
#6704=CARTESIAN_POINT('',(-1.,0.,0.));
#6705=CARTESIAN_POINT('',(-1.,-0.3,0.04));
#6706=CARTESIAN_POINT('',(-1.,-0.2925,0.0325));
#6707=CARTESIAN_POINT('',(-1.,-0.3,0.175));
#6708=CARTESIAN_POINT('Origin',(0.75,0.28,0.02));
#6709=CARTESIAN_POINT('',(1.,0.3,0.04));
#6710=CARTESIAN_POINT('',(0.75,0.3,0.04));
#6711=CARTESIAN_POINT('',(1.,0.26,0.));
#6712=CARTESIAN_POINT('',(1.,0.2925,0.0325));
#6713=CARTESIAN_POINT('',(0.75,0.26,0.));
#6714=CARTESIAN_POINT('Origin',(1.5,0.3,0.));
#6715=CARTESIAN_POINT('',(1.,0.3,0.56));
#6716=CARTESIAN_POINT('',(0.75,0.3,0.56));
#6717=CARTESIAN_POINT('',(1.,0.3,0.175));
#6718=CARTESIAN_POINT('Origin',(0.75,0.28,0.58));
#6719=CARTESIAN_POINT('',(1.,0.26,0.6));
#6720=CARTESIAN_POINT('',(0.75,0.26,0.6));
#6721=CARTESIAN_POINT('',(1.,0.2675,0.5925));
#6722=CARTESIAN_POINT('Origin',(0.,0.,0.6));
#6723=CARTESIAN_POINT('',(1.,-0.26,0.6));
#6724=CARTESIAN_POINT('',(-0.75,-0.26,0.6));
#6725=CARTESIAN_POINT('',(1.,0.,0.6));
#6726=CARTESIAN_POINT('Origin',(1.,0.,0.35));
#6727=CARTESIAN_POINT('',(1.,-0.26,0.));
#6728=CARTESIAN_POINT('',(1.,-0.3,0.04));
#6729=CARTESIAN_POINT('',(1.,-0.2925,0.0325));
#6730=CARTESIAN_POINT('',(1.,0.,0.));
#6731=CARTESIAN_POINT('',(1.,-0.3,0.56));
#6732=CARTESIAN_POINT('',(1.,-0.2675,0.5925));
#6733=CARTESIAN_POINT('',(1.,-0.3,0.175));
#6734=CARTESIAN_POINT('Origin',(0.,0.,0.));
#6735=CARTESIAN_POINT('',(-0.75,-0.26,0.));
#6736=CARTESIAN_POINT('Origin',(-0.75,-0.28,0.58));
#6737=CARTESIAN_POINT('',(-0.75,-0.3,0.56));
#6738=CARTESIAN_POINT('Origin',(-0.75,-0.28,0.02));
#6739=CARTESIAN_POINT('',(-0.75,-0.3,0.04));
#6740=CARTESIAN_POINT('Origin',(-1.5,-0.3,0.));
#6741=CARTESIAN_POINT('',(0.,0.,0.));
#6742=CARTESIAN_POINT('Origin',(0.45,0.6,0.));
#6743=CARTESIAN_POINT('',(-0.45,0.6,-5.51091059616309E-17));
#6744=CARTESIAN_POINT('Origin',(0.,0.6,0.));
#6745=CARTESIAN_POINT('Origin',(0.,0.575,0.));
#6746=CARTESIAN_POINT('',(-0.5,0.55,-6.12323399573677E-17));
#6747=CARTESIAN_POINT('Origin',(0.,0.55,0.));
#6748=CARTESIAN_POINT('',(-0.475,0.575,-5.81707229594993E-17));
#6749=CARTESIAN_POINT('Origin',(0.,0.29,0.));
#6750=CARTESIAN_POINT('',(-0.5,0.0299999999999998,-6.12323399573677E-17));
#6751=CARTESIAN_POINT('Origin',(0.,0.0299999999999998,0.));
#6752=CARTESIAN_POINT('',(-0.5,0.29,-6.12323399573677E-17));
#6753=CARTESIAN_POINT('Origin',(0.,0.0150000000000001,0.));
#6754=CARTESIAN_POINT('',(-0.47,7.11236625150491E-17,-5.75583995599256E-17));
#6755=CARTESIAN_POINT('Origin',(0.,0.,0.));
#6756=CARTESIAN_POINT('',(-0.485,0.0150000000000001,-5.93953697586466E-17));
#6757=CARTESIAN_POINT('Origin',(0.32,0.,0.));
#6758=CARTESIAN_POINT('',(-0.32,-6.93889390390723E-18,-3.91886975727153E-17));
#6759=CARTESIAN_POINT('Origin',(0.,0.,0.));
#6760=CARTESIAN_POINT('Origin',(0.,-0.02,0.));
#6761=CARTESIAN_POINT('',(-0.2942,-0.0515999999999999,3.60291088309151E-17));
#6762=CARTESIAN_POINT('Origin',(0.,-0.0515999999999999,0.));
#6763=CARTESIAN_POINT('',(-0.31,-0.02,-3.7964050773568E-17));
#6764=CARTESIAN_POINT('Origin',(0.,-1.24,0.));
#6765=CARTESIAN_POINT('',(-0.2942,-2.4458,3.60291088309151E-17));
#6766=CARTESIAN_POINT('Origin',(0.,-2.4458,0.));
#6767=CARTESIAN_POINT('',(-0.2942,-1.24,-3.60291088309151E-17));
#6768=CARTESIAN_POINT('Origin',(0.,-2.47,0.));
#6769=CARTESIAN_POINT('',(-0.24,-2.5,-2.93915231795365E-17));
#6770=CARTESIAN_POINT('Origin',(0.,-2.5,0.));
#6771=CARTESIAN_POINT('',(-0.27,-2.47,-3.30654635769785E-17));
#6772=CARTESIAN_POINT('Origin',(0.,-2.5,0.));
#6773=CARTESIAN_POINT('Origin',(0.144337567297406,-0.6,-0.25));
#6774=CARTESIAN_POINT('',(0.288675134594813,-0.6,0.));
#6775=CARTESIAN_POINT('',(0.144337567297406,-0.6,-0.25));
#6776=CARTESIAN_POINT('',(0.288675134594813,-0.6,0.));
#6777=CARTESIAN_POINT('',(0.144337567297406,-0.96,-0.25));
#6778=CARTESIAN_POINT('',(0.144337567297406,-0.6,-0.25));
#6779=CARTESIAN_POINT('',(0.288675134594813,-0.96,0.));
#6780=CARTESIAN_POINT('',(0.288675134594813,-0.96,0.));
#6781=CARTESIAN_POINT('',(0.288675134594813,-0.6,0.));
#6782=CARTESIAN_POINT('Origin',(-0.144337567297406,-0.6,-0.25));
#6783=CARTESIAN_POINT('',(-0.144337567297406,-0.6,-0.25));
#6784=CARTESIAN_POINT('',(0.144337567297406,-0.6,-0.25));
#6785=CARTESIAN_POINT('',(-0.144337567297406,-0.96,-0.25));
#6786=CARTESIAN_POINT('',(-0.144337567297406,-0.6,-0.25));
#6787=CARTESIAN_POINT('',(0.144337567297406,-0.96,-0.25));
#6788=CARTESIAN_POINT('Origin',(-0.288675134594813,-0.6,-8.32667268468867E-17));
#6789=CARTESIAN_POINT('',(-0.288675134594813,-0.6,-3.53525079574969E-17));
#6790=CARTESIAN_POINT('',(-0.144337567297406,-0.6,-0.25));
#6791=CARTESIAN_POINT('',(-0.288675134594813,-0.96,-5.55111512312578E-17));
#6792=CARTESIAN_POINT('',(-0.288675134594813,-0.6,-3.53525079574969E-17));
#6793=CARTESIAN_POINT('',(-0.144337567297406,-0.96,-0.25));
#6794=CARTESIAN_POINT('Origin',(-0.144337567297407,-0.6,0.25));
#6795=CARTESIAN_POINT('',(-0.144337567297407,-0.6,0.25));
#6796=CARTESIAN_POINT('',(-0.288675134594813,-0.6,-3.53525079574969E-17));
#6797=CARTESIAN_POINT('',(-0.144337567297407,-0.96,0.25));
#6798=CARTESIAN_POINT('',(-0.144337567297407,-0.6,0.25));
#6799=CARTESIAN_POINT('',(-0.288675134594813,-0.96,-3.53525079574969E-17));
#6800=CARTESIAN_POINT('Origin',(0.144337567297406,-0.6,0.25));
#6801=CARTESIAN_POINT('',(0.144337567297406,-0.6,0.25));
#6802=CARTESIAN_POINT('',(-0.144337567297407,-0.6,0.25));
#6803=CARTESIAN_POINT('',(0.144337567297406,-0.96,0.25));
#6804=CARTESIAN_POINT('',(0.144337567297406,-0.6,0.25));
#6805=CARTESIAN_POINT('',(-0.144337567297407,-0.96,0.25));
#6806=CARTESIAN_POINT('Origin',(0.288675134594813,-0.6,0.));
#6807=CARTESIAN_POINT('',(0.144337567297406,-0.6,0.25));
#6808=CARTESIAN_POINT('',(0.144337567297406,-0.96,0.25));
#6809=CARTESIAN_POINT('Origin',(0.,-0.6,0.));
#6810=CARTESIAN_POINT('Origin',(0.,-0.96,0.));
#6811=CARTESIAN_POINT('',(0.,0.,0.));
#6812=CARTESIAN_POINT('Origin',(0.375,0.5,0.));
#6813=CARTESIAN_POINT('',(-0.375,0.5,-4.59242549680257E-17));
#6814=CARTESIAN_POINT('Origin',(0.,0.5,0.));
#6815=CARTESIAN_POINT('Origin',(0.,0.475,0.));
#6816=CARTESIAN_POINT('',(-0.425,0.45,-5.20474889637625E-17));
#6817=CARTESIAN_POINT('Origin',(0.,0.45,0.));
#6818=CARTESIAN_POINT('',(-0.4,0.475,-4.89858719658941E-17));
#6819=CARTESIAN_POINT('Origin',(0.,0.24,0.));
#6820=CARTESIAN_POINT('',(-0.425,0.0299999999999998,-5.20474889637625E-17));
#6821=CARTESIAN_POINT('Origin',(0.,0.0299999999999998,0.));
#6822=CARTESIAN_POINT('',(-0.425,0.24,-5.20474889637625E-17));
#6823=CARTESIAN_POINT('Origin',(0.,0.0150000000000001,0.));
#6824=CARTESIAN_POINT('',(-0.395,4.85722573273506E-17,-4.83735485663204E-17));
#6825=CARTESIAN_POINT('Origin',(0.,0.,0.));
#6826=CARTESIAN_POINT('',(-0.41,0.0150000000000001,-5.02105187650415E-17));
#6827=CARTESIAN_POINT('Origin',(0.27,0.,0.));
#6828=CARTESIAN_POINT('',(-0.27,0.,-3.30654635769785E-17));
#6829=CARTESIAN_POINT('Origin',(0.,0.,0.));
#6830=CARTESIAN_POINT('Origin',(0.,-0.02,0.));
#6831=CARTESIAN_POINT('',(-0.24505,-0.0498999999999999,3.00099698131059E-17));
#6832=CARTESIAN_POINT('Origin',(0.,-0.0498999999999999,0.));
#6833=CARTESIAN_POINT('',(-0.26,-0.02,-3.18408167778312E-17));
#6834=CARTESIAN_POINT('Origin',(0.,-0.995,0.));
#6835=CARTESIAN_POINT('',(-0.24505,-1.95495,3.00099698131059E-17));
#6836=CARTESIAN_POINT('Origin',(0.,-1.95495,0.));
#6837=CARTESIAN_POINT('',(-0.24505,-0.995,-3.00099698131059E-17));
#6838=CARTESIAN_POINT('Origin',(0.,-1.975,0.));
#6839=CARTESIAN_POINT('',(-0.2,-2.,-2.44929359829471E-17));
#6840=CARTESIAN_POINT('Origin',(0.,-2.,0.));
#6841=CARTESIAN_POINT('',(-0.225,-1.975,-2.75545529808154E-17));
#6842=CARTESIAN_POINT('Origin',(0.,-2.,0.));
#6843=CARTESIAN_POINT('Origin',(0.115470053837925,-0.5,-0.2));
#6844=CARTESIAN_POINT('',(0.23094010767585,-0.5,0.));
#6845=CARTESIAN_POINT('',(0.115470053837925,-0.5,-0.2));
#6846=CARTESIAN_POINT('',(0.23094010767585,-0.5,0.));
#6847=CARTESIAN_POINT('',(0.115470053837925,-0.8,-0.2));
#6848=CARTESIAN_POINT('',(0.115470053837925,-0.5,-0.2));
#6849=CARTESIAN_POINT('',(0.23094010767585,-0.8,0.));
#6850=CARTESIAN_POINT('',(0.23094010767585,-0.8,0.));
#6851=CARTESIAN_POINT('',(0.23094010767585,-0.5,0.));
#6852=CARTESIAN_POINT('Origin',(-0.115470053837925,-0.5,-0.2));
#6853=CARTESIAN_POINT('',(-0.115470053837925,-0.5,-0.2));
#6854=CARTESIAN_POINT('',(0.115470053837925,-0.5,-0.2));
#6855=CARTESIAN_POINT('',(-0.115470053837925,-0.8,-0.2));
#6856=CARTESIAN_POINT('',(-0.115470053837925,-0.5,-0.2));
#6857=CARTESIAN_POINT('',(0.115470053837925,-0.8,-0.2));
#6858=CARTESIAN_POINT('Origin',(-0.23094010767585,-0.5,-2.77555756156289E-17));
#6859=CARTESIAN_POINT('',(-0.23094010767585,-0.5,-2.82820063659975E-17));
#6860=CARTESIAN_POINT('',(-0.115470053837925,-0.5,-0.2));
#6861=CARTESIAN_POINT('',(-0.23094010767585,-0.8,-2.77555756156289E-17));
#6862=CARTESIAN_POINT('',(-0.23094010767585,-0.5,-2.82820063659975E-17));
#6863=CARTESIAN_POINT('',(-0.115470053837925,-0.8,-0.2));
#6864=CARTESIAN_POINT('Origin',(-0.115470053837925,-0.5,0.2));
#6865=CARTESIAN_POINT('',(-0.115470053837925,-0.5,0.2));
#6866=CARTESIAN_POINT('',(-0.23094010767585,-0.5,-2.82820063659975E-17));
#6867=CARTESIAN_POINT('',(-0.115470053837925,-0.8,0.2));
#6868=CARTESIAN_POINT('',(-0.115470053837925,-0.5,0.2));
#6869=CARTESIAN_POINT('',(-0.23094010767585,-0.8,-2.82820063659975E-17));
#6870=CARTESIAN_POINT('Origin',(0.115470053837925,-0.5,0.2));
#6871=CARTESIAN_POINT('',(0.115470053837925,-0.5,0.2));
#6872=CARTESIAN_POINT('',(-0.115470053837925,-0.5,0.2));
#6873=CARTESIAN_POINT('',(0.115470053837925,-0.8,0.2));
#6874=CARTESIAN_POINT('',(0.115470053837925,-0.5,0.2));
#6875=CARTESIAN_POINT('',(-0.115470053837925,-0.8,0.2));
#6876=CARTESIAN_POINT('Origin',(0.23094010767585,-0.5,0.));
#6877=CARTESIAN_POINT('',(0.115470053837925,-0.5,0.2));
#6878=CARTESIAN_POINT('',(0.115470053837925,-0.8,0.2));
#6879=CARTESIAN_POINT('Origin',(0.,-0.5,0.));
#6880=CARTESIAN_POINT('Origin',(0.,-0.8,0.));
#6881=CARTESIAN_POINT('',(0.,0.,0.));
#6882=CARTESIAN_POINT('Origin',(0.,0.,0.));
#6883=CARTESIAN_POINT('',(-0.265,0.1,3.24531401774049E-17));
#6884=CARTESIAN_POINT('Origin',(0.,0.1,0.));
#6885=CARTESIAN_POINT('',(-0.265,0.,3.24531401774049E-17));
#6886=CARTESIAN_POINT('',(-0.265,0.,3.24531401774049E-17));
#6887=CARTESIAN_POINT('Origin',(0.,0.,0.));
#6888=CARTESIAN_POINT('Origin',(0.,0.,0.));
#6889=CARTESIAN_POINT('',(-0.5,0.1,6.12323399573677E-17));
#6890=CARTESIAN_POINT('Origin',(0.,0.1,0.));
#6891=CARTESIAN_POINT('',(-0.5,0.,6.12323399573677E-17));
#6892=CARTESIAN_POINT('',(-0.5,0.,6.12323399573677E-17));
#6893=CARTESIAN_POINT('Origin',(0.,0.,0.));
#6894=CARTESIAN_POINT('Origin',(0.,0.1,0.));
#6895=CARTESIAN_POINT('Origin',(0.,0.,0.));
#6896=CARTESIAN_POINT('',(0.,0.,0.));
#6897=CARTESIAN_POINT('Origin',(0.,0.0525042956467857,0.));
#6898=CARTESIAN_POINT('',(-0.230940107675851,0.0472735643746089,0.4));
#6899=CARTESIAN_POINT('',(0.23094010767585,0.0472735643746089,0.4));
#6900=CARTESIAN_POINT('Ctrl Pts',(-0.230940107675851,0.0472735643746089,
0.4));
#6901=CARTESIAN_POINT('Ctrl Pts',(1.11022302462516E-16,-0.0193931022920578,
0.4));
#6902=CARTESIAN_POINT('Ctrl Pts',(0.23094010767585,0.0472735643746089,0.4));
#6903=CARTESIAN_POINT('',(-0.461880215351701,0.0472735643746089,-5.6564012731995E-17));
#6904=CARTESIAN_POINT('Ctrl Pts',(-0.461880215351701,0.0472735643746089,
-5.6564012731995E-17));
#6905=CARTESIAN_POINT('Ctrl Pts',(-0.346410161513776,-0.0193931022920579,
0.2));
#6906=CARTESIAN_POINT('Ctrl Pts',(-0.230940107675851,0.0472735643746089,
0.4));
#6907=CARTESIAN_POINT('',(-0.38,-2.08166817117217E-17,-4.65365783675994E-17));
#6908=CARTESIAN_POINT('',(-0.47094010767585,0.0525042956467857,-5.7673529545534E-17));
#6909=CARTESIAN_POINT('Origin',(0.,0.,0.));
#6910=CARTESIAN_POINT('',(-0.23094010767585,0.0472735643746089,-0.4));
#6911=CARTESIAN_POINT('Ctrl Pts',(-0.23094010767585,0.0472735643746089,
-0.4));
#6912=CARTESIAN_POINT('Ctrl Pts',(-0.346410161513775,-0.0193931022920578,
-0.2));
#6913=CARTESIAN_POINT('Ctrl Pts',(-0.461880215351701,0.0472735643746089,
-5.6564012731995E-17));
#6914=CARTESIAN_POINT('',(0.23094010767585,0.0472735643746089,-0.4));
#6915=CARTESIAN_POINT('Ctrl Pts',(0.23094010767585,0.0472735643746089,-0.4));
#6916=CARTESIAN_POINT('Ctrl Pts',(0.,-0.0193931022920578,-0.4));
#6917=CARTESIAN_POINT('Ctrl Pts',(-0.23094010767585,0.0472735643746089,
-0.4));
#6918=CARTESIAN_POINT('',(0.461880215351701,0.0472735643746089,0.));
#6919=CARTESIAN_POINT('Ctrl Pts',(0.461880215351701,0.0472735643746089,
0.));
#6920=CARTESIAN_POINT('Ctrl Pts',(0.346410161513776,-0.019393102292058,
-0.2));
#6921=CARTESIAN_POINT('Ctrl Pts',(0.23094010767585,0.0472735643746089,-0.4));
#6922=CARTESIAN_POINT('Ctrl Pts',(0.23094010767585,0.0472735643746089,0.4));
#6923=CARTESIAN_POINT('Ctrl Pts',(0.346410161513776,-0.0193931022920577,
0.2));
#6924=CARTESIAN_POINT('Ctrl Pts',(0.461880215351701,0.0472735643746089,
0.));
#6925=CARTESIAN_POINT('Origin',(0.,0.417495704353214,0.));
#6926=CARTESIAN_POINT('',(-0.38,0.47,-4.65365783675994E-17));
#6927=CARTESIAN_POINT('Origin',(0.,0.47,0.));
#6928=CARTESIAN_POINT('',(-0.461880215351701,0.422726435625391,-5.6564012731995E-17));
#6929=CARTESIAN_POINT('',(-0.47094010767585,0.417495704353214,-5.7673529545534E-17));
#6930=CARTESIAN_POINT('',(-0.230940107675851,0.422726435625391,0.4));
#6931=CARTESIAN_POINT('Ctrl Pts',(-0.230940107675851,0.422726435625391,
0.4));
#6932=CARTESIAN_POINT('Ctrl Pts',(-0.346410161513776,0.489393102292058,
0.2));
#6933=CARTESIAN_POINT('Ctrl Pts',(-0.461880215351701,0.422726435625391,
-5.6564012731995E-17));
#6934=CARTESIAN_POINT('',(0.23094010767585,0.422726435625391,0.4));
#6935=CARTESIAN_POINT('Ctrl Pts',(0.23094010767585,0.422726435625391,0.4));
#6936=CARTESIAN_POINT('Ctrl Pts',(8.32667268468867E-17,0.489393102292058,
0.4));
#6937=CARTESIAN_POINT('Ctrl Pts',(-0.230940107675851,0.422726435625391,
0.4));
#6938=CARTESIAN_POINT('',(0.461880215351701,0.422726435625391,0.));
#6939=CARTESIAN_POINT('Ctrl Pts',(0.461880215351701,0.422726435625391,0.));
#6940=CARTESIAN_POINT('Ctrl Pts',(0.346410161513776,0.489393102292058,0.2));
#6941=CARTESIAN_POINT('Ctrl Pts',(0.23094010767585,0.422726435625391,0.4));
#6942=CARTESIAN_POINT('',(0.23094010767585,0.422726435625391,-0.4));
#6943=CARTESIAN_POINT('Ctrl Pts',(0.23094010767585,0.422726435625391,-0.4));
#6944=CARTESIAN_POINT('Ctrl Pts',(0.346410161513775,0.489393102292058,-0.2));
#6945=CARTESIAN_POINT('Ctrl Pts',(0.461880215351701,0.422726435625391,0.));
#6946=CARTESIAN_POINT('',(-0.23094010767585,0.422726435625391,-0.4));
#6947=CARTESIAN_POINT('Ctrl Pts',(-0.23094010767585,0.422726435625391,-0.4));
#6948=CARTESIAN_POINT('Ctrl Pts',(-5.55111512312578E-17,0.489393102292058,
-0.4));
#6949=CARTESIAN_POINT('Ctrl Pts',(0.23094010767585,0.422726435625391,-0.4));
#6950=CARTESIAN_POINT('Ctrl Pts',(-0.461880215351701,0.422726435625391,
-5.6564012731995E-17));
#6951=CARTESIAN_POINT('Ctrl Pts',(-0.346410161513776,0.489393102292058,
-0.2));
#6952=CARTESIAN_POINT('Ctrl Pts',(-0.23094010767585,0.422726435625391,-0.4));
#6953=CARTESIAN_POINT('Origin',(0.23094010767585,0.,-0.4));
#6954=CARTESIAN_POINT('',(-0.23094010767585,0.,-0.4));
#6955=CARTESIAN_POINT('',(0.23094010767585,0.,-0.4));
#6956=CARTESIAN_POINT('Origin',(-0.23094010767585,0.,-0.4));
#6957=CARTESIAN_POINT('',(-0.461880215351701,0.,-5.6564012731995E-17));
#6958=CARTESIAN_POINT('Origin',(-0.461880215351701,0.,-5.6564012731995E-17));
#6959=CARTESIAN_POINT('',(-0.230940107675851,0.,0.4));
#6960=CARTESIAN_POINT('Origin',(0.,0.,0.));
#6961=CARTESIAN_POINT('',(-0.2117,0.47,2.59257727379495E-17));
#6962=CARTESIAN_POINT('Origin',(0.,0.47,0.));
#6963=CARTESIAN_POINT('',(-0.2117,0.,2.59257727379495E-17));
#6964=CARTESIAN_POINT('',(-0.2117,0.,2.59257727379495E-17));
#6965=CARTESIAN_POINT('Origin',(0.,0.,0.));
#6966=CARTESIAN_POINT('Origin',(-0.230940107675851,0.,0.4));
#6967=CARTESIAN_POINT('',(0.23094010767585,0.,0.4));
#6968=CARTESIAN_POINT('Origin',(0.461880215351701,0.,0.));
#6969=CARTESIAN_POINT('',(0.461880215351701,0.,0.));
#6970=CARTESIAN_POINT('Origin',(0.23094010767585,0.,0.4));
#6971=CARTESIAN_POINT('Origin',(0.,0.47,0.));
#6972=CARTESIAN_POINT('Origin',(0.,0.,0.));
#6973=CARTESIAN_POINT('',(0.,0.,0.));
#6974=CARTESIAN_POINT('',(0.,0.,0.));
#6975=CARTESIAN_POINT('',(0.,0.,0.));
#6976=CARTESIAN_POINT('',(0.,0.,0.));
#6977=CARTESIAN_POINT('',(0.,0.,0.));
#6978=CARTESIAN_POINT('',(0.,0.,0.));
#6979=CARTESIAN_POINT('',(0.,0.,0.));
#6980=CARTESIAN_POINT('',(0.,0.,0.));
#6981=CARTESIAN_POINT('',(3.,-4.5,1.));
#6982=CARTESIAN_POINT('',(3.,4.5,1.));
#6983=CARTESIAN_POINT('',(17.,-4.5,1.));
#6984=CARTESIAN_POINT('',(17.,4.5,1.));
#6985=CARTESIAN_POINT('',(6.5,-2.5,2.5));
#6986=CARTESIAN_POINT('',(6.5,2.5,2.5));
#6987=CARTESIAN_POINT('',(6.5,0.,0.7));
#6988=CARTESIAN_POINT('',(13.5,-2.5,2.5));
#6989=CARTESIAN_POINT('',(13.5,2.5,2.5));
#6990=CARTESIAN_POINT('',(13.5,0.,0.7));
#6991=CARTESIAN_POINT('',(2.,-1.4,2.5));
#6992=CARTESIAN_POINT('',(2.,1.4,2.5));
#6993=CARTESIAN_POINT('',(1.,0.,4.62132034355964));
#6994=CARTESIAN_POINT('',(1.5,0.,4.62132034355964));
#6995=CARTESIAN_POINT('',(1.4,0.,4.62132034355964));
#6996=CARTESIAN_POINT('',(0.,0.,0.));
#6997=CARTESIAN_POINT('',(0.,0.,0.));
#6998=CARTESIAN_POINT('Origin',(10.,-0.8,6.42132034));
#6999=CARTESIAN_POINT('',(9.775,-0.8,6.52132034));
#7000=CARTESIAN_POINT('Origin',(10.,-0.8,6.52132034));
#7001=CARTESIAN_POINT('',(9.775,-0.8,7.12132034));
#7002=CARTESIAN_POINT('',(9.775,-0.8,6.42132034));
#7003=CARTESIAN_POINT('Origin',(10.,-0.8,7.12132034));
#7004=CARTESIAN_POINT('Origin',(10.,0.8,6.42132034));
#7005=CARTESIAN_POINT('',(9.775,0.8,6.52132034));
#7006=CARTESIAN_POINT('Origin',(10.,0.8,6.52132034));
#7007=CARTESIAN_POINT('',(9.775,0.8,7.12132034));
#7008=CARTESIAN_POINT('',(9.775,0.8,6.42132034));
#7009=CARTESIAN_POINT('Origin',(10.,0.8,7.12132034));
#7010=CARTESIAN_POINT('Origin',(10.,-4.,6.42132034));
#7011=CARTESIAN_POINT('',(9.55,-4.,6.52132034));
#7012=CARTESIAN_POINT('Origin',(10.,-4.,6.52132034));
#7013=CARTESIAN_POINT('',(9.55,-4.,7.12132034));
#7014=CARTESIAN_POINT('',(9.55,-4.,6.42132034));
#7015=CARTESIAN_POINT('Origin',(10.,-4.,7.12132034));
#7016=CARTESIAN_POINT('Origin',(10.,4.,6.42132034));
#7017=CARTESIAN_POINT('',(9.55,4.,6.52132034));
#7018=CARTESIAN_POINT('Origin',(10.,4.,6.52132034));
#7019=CARTESIAN_POINT('',(9.55,4.,7.12132034));
#7020=CARTESIAN_POINT('',(9.55,4.,6.42132034));
#7021=CARTESIAN_POINT('Origin',(10.,4.,7.12132034));
#7022=CARTESIAN_POINT('Origin',(11.,4.7,6.52132034));
#7023=CARTESIAN_POINT('',(11.,4.7,6.52132034));
#7024=CARTESIAN_POINT('',(9.,4.7,6.52132034));
#7025=CARTESIAN_POINT('',(11.,4.7,6.52132034));
#7026=CARTESIAN_POINT('',(9.,4.7,7.12132034));
#7027=CARTESIAN_POINT('',(9.,4.7,6.52132034));
#7028=CARTESIAN_POINT('',(11.,4.7,7.12132034));
#7029=CARTESIAN_POINT('',(11.,4.7,7.12132034));
#7030=CARTESIAN_POINT('',(11.,4.7,6.52132034));
#7031=CARTESIAN_POINT('Origin',(11.,-4.7,6.52132034));
#7032=CARTESIAN_POINT('',(11.,-4.7,6.52132034));
#7033=CARTESIAN_POINT('',(11.,-4.7,6.52132034));
#7034=CARTESIAN_POINT('',(11.,-4.7,7.12132034));
#7035=CARTESIAN_POINT('',(11.,-4.7,7.12132034));
#7036=CARTESIAN_POINT('',(11.,-4.7,6.52132034));
#7037=CARTESIAN_POINT('Origin',(9.,-4.7,6.52132034));
#7038=CARTESIAN_POINT('',(9.,-4.7,6.52132034));
#7039=CARTESIAN_POINT('',(9.,-4.7,6.52132034));
#7040=CARTESIAN_POINT('',(9.,-4.7,7.12132034));
#7041=CARTESIAN_POINT('',(9.,-4.7,7.12132034));
#7042=CARTESIAN_POINT('',(9.,-4.7,6.52132034));
#7043=CARTESIAN_POINT('Origin',(9.,4.7,6.52132034));
#7044=CARTESIAN_POINT('',(9.,4.7,6.52132034));
#7045=CARTESIAN_POINT('',(9.,4.7,7.12132034));
#7046=CARTESIAN_POINT('Origin',(10.,0.,7.12132034));
#7047=CARTESIAN_POINT('Origin',(10.,0.,6.52132034));
#7048=CARTESIAN_POINT('',(0.,0.,0.));
#7049=CARTESIAN_POINT('Origin',(10.,-0.8,6.02132034));
#7050=CARTESIAN_POINT('',(9.835,-0.8,6.02132034));
#7051=CARTESIAN_POINT('Origin',(10.,-0.8,6.02132034));
#7052=CARTESIAN_POINT('',(9.835,-0.8,6.52132034));
#7053=CARTESIAN_POINT('',(9.835,-0.8,6.02132034));
#7054=CARTESIAN_POINT('Origin',(10.,-0.8,6.52132034));
#7055=CARTESIAN_POINT('Origin',(10.,-0.8,6.02132034));
#7056=CARTESIAN_POINT('Origin',(10.,0.8,6.02132034));
#7057=CARTESIAN_POINT('',(9.835,0.8,6.02132034));
#7058=CARTESIAN_POINT('Origin',(10.,0.8,6.02132034));
#7059=CARTESIAN_POINT('',(9.835,0.8,6.52132034));
#7060=CARTESIAN_POINT('',(9.835,0.8,6.02132034));
#7061=CARTESIAN_POINT('Origin',(10.,0.8,6.52132034));
#7062=CARTESIAN_POINT('Origin',(10.,0.8,6.02132034));
#7063=CARTESIAN_POINT('Origin',(8.9,0.,4.62132034355964));
#7064=CARTESIAN_POINT('',(11.,1.2,5.52132034));
#7065=CARTESIAN_POINT('',(9.,1.2,5.52132034));
#7066=CARTESIAN_POINT('',(11.,1.2,5.52132034));
#7067=CARTESIAN_POINT('',(11.,-1.2,5.52132034));
#7068=CARTESIAN_POINT('Origin',(11.,0.,4.62132034355964));
#7069=CARTESIAN_POINT('',(9.,-1.2,5.52132034));
#7070=CARTESIAN_POINT('',(9.,-1.2,5.52132034));
#7071=CARTESIAN_POINT('Origin',(9.,0.,4.62132034355964));
#7072=CARTESIAN_POINT('Origin',(11.,-1.2,5.52132034));
#7073=CARTESIAN_POINT('',(11.,1.2,6.52132034));
#7074=CARTESIAN_POINT('',(11.,1.2,5.52132034));
#7075=CARTESIAN_POINT('',(11.,-1.2,6.52132034));
#7076=CARTESIAN_POINT('',(11.,-1.2,6.52132034));
#7077=CARTESIAN_POINT('',(11.,-1.2,5.52132034));
#7078=CARTESIAN_POINT('Origin',(11.,1.2,5.52132034));
#7079=CARTESIAN_POINT('',(9.,1.2,6.52132034));
#7080=CARTESIAN_POINT('',(9.,1.2,5.52132034));
#7081=CARTESIAN_POINT('',(11.,1.2,6.52132034));
#7082=CARTESIAN_POINT('Origin',(9.,-1.2,5.52132034));
#7083=CARTESIAN_POINT('',(9.,-1.2,6.52132034));
#7084=CARTESIAN_POINT('',(9.,-1.2,6.52132034));
#7085=CARTESIAN_POINT('',(9.,-1.2,5.52132034));
#7086=CARTESIAN_POINT('Origin',(9.,1.2,5.52132034));
#7087=CARTESIAN_POINT('',(9.,1.2,6.52132034));
#7088=CARTESIAN_POINT('Origin',(10.,0.,6.52132034));
#7089=CARTESIAN_POINT('',(0.,0.,0.));
#7090=CARTESIAN_POINT('Origin',(10.,-4.,0.));
#7091=CARTESIAN_POINT('',(9.6067,-4.,8.3));
#7092=CARTESIAN_POINT('Origin',(10.,-4.,8.3));
#7093=CARTESIAN_POINT('',(9.6067,-4.,0.));
#7094=CARTESIAN_POINT('',(9.6067,-4.,0.));
#7095=CARTESIAN_POINT('Origin',(10.,-4.,0.));
#7096=CARTESIAN_POINT('Origin',(10.,-4.,8.3));
#7097=CARTESIAN_POINT('Origin',(10.,-4.,0.));
#7098=CARTESIAN_POINT('',(0.,0.,0.));
#7099=CARTESIAN_POINT('Origin',(10.,4.,0.));
#7100=CARTESIAN_POINT('',(9.6067,4.,8.3));
#7101=CARTESIAN_POINT('Origin',(10.,4.,8.3));
#7102=CARTESIAN_POINT('',(9.6067,4.,0.));
#7103=CARTESIAN_POINT('',(9.6067,4.,0.));
#7104=CARTESIAN_POINT('Origin',(10.,4.,0.));
#7105=CARTESIAN_POINT('Origin',(10.,4.,8.3));
#7106=CARTESIAN_POINT('Origin',(10.,4.,0.));
#7107=CARTESIAN_POINT('',(0.,0.,0.));
#7108=CARTESIAN_POINT('Origin',(0.0866025403784439,-0.4,-0.15));
#7109=CARTESIAN_POINT('',(0.173205080756888,-0.4,0.));
#7110=CARTESIAN_POINT('',(0.0866025403784439,-0.4,-0.15));
#7111=CARTESIAN_POINT('',(0.173205080756888,-0.4,0.));
#7112=CARTESIAN_POINT('',(0.0866025403784439,-0.64,-0.15));
#7113=CARTESIAN_POINT('',(0.0866025403784439,-0.4,-0.15));
#7114=CARTESIAN_POINT('',(0.173205080756888,-0.64,0.));
#7115=CARTESIAN_POINT('',(0.173205080756888,-0.64,0.));
#7116=CARTESIAN_POINT('',(0.173205080756888,-0.4,0.));
#7117=CARTESIAN_POINT('Origin',(-0.0866025403784438,-0.4,-0.15));
#7118=CARTESIAN_POINT('',(-0.0866025403784438,-0.4,-0.15));
#7119=CARTESIAN_POINT('',(0.0866025403784439,-0.4,-0.15));
#7120=CARTESIAN_POINT('',(-0.0866025403784438,-0.64,-0.15));
#7121=CARTESIAN_POINT('',(-0.0866025403784438,-0.4,-0.15));
#7122=CARTESIAN_POINT('',(0.0866025403784439,-0.64,-0.15));
#7123=CARTESIAN_POINT('Origin',(-0.173205080756888,-0.4,-2.77555756156289E-17));
#7124=CARTESIAN_POINT('',(-0.173205080756888,-0.4,-2.12115047744981E-17));
#7125=CARTESIAN_POINT('',(-0.0866025403784438,-0.4,-0.15));
#7126=CARTESIAN_POINT('',(-0.173205080756888,-0.64,-2.77555756156289E-17));
#7127=CARTESIAN_POINT('',(-0.173205080756888,-0.4,-2.12115047744981E-17));
#7128=CARTESIAN_POINT('',(-0.0866025403784438,-0.64,-0.15));
#7129=CARTESIAN_POINT('Origin',(-0.0866025403784439,-0.4,0.15));
#7130=CARTESIAN_POINT('',(-0.0866025403784439,-0.4,0.15));
#7131=CARTESIAN_POINT('',(-0.173205080756888,-0.4,-2.12115047744981E-17));
#7132=CARTESIAN_POINT('',(-0.0866025403784439,-0.64,0.15));
#7133=CARTESIAN_POINT('',(-0.0866025403784439,-0.4,0.15));
#7134=CARTESIAN_POINT('',(-0.173205080756888,-0.64,-2.12115047744981E-17));
#7135=CARTESIAN_POINT('Origin',(0.0866025403784439,-0.4,0.15));
#7136=CARTESIAN_POINT('',(0.0866025403784439,-0.4,0.15));
#7137=CARTESIAN_POINT('',(-0.0866025403784439,-0.4,0.15));
#7138=CARTESIAN_POINT('',(0.0866025403784439,-0.64,0.15));
#7139=CARTESIAN_POINT('',(0.0866025403784439,-0.4,0.15));
#7140=CARTESIAN_POINT('',(-0.0866025403784439,-0.64,0.15));
#7141=CARTESIAN_POINT('Origin',(0.173205080756888,-0.4,0.));
#7142=CARTESIAN_POINT('',(0.0866025403784439,-0.4,0.15));
#7143=CARTESIAN_POINT('',(0.0866025403784439,-0.64,0.15));
#7144=CARTESIAN_POINT('Origin',(0.,-0.4,-2.77555756156289E-17));
#7145=CARTESIAN_POINT('Origin',(0.,-0.64,-2.77555756156289E-17));
#7146=CARTESIAN_POINT('Origin',(0.,-1.,0.));
#7147=CARTESIAN_POINT('',(-0.1954,-1.,2.39295984553393E-17));
#7148=CARTESIAN_POINT('Origin',(0.,-1.,0.));
#7149=CARTESIAN_POINT('Origin',(0.3,0.4,0.));
#7150=CARTESIAN_POINT('',(-0.3,0.4,-3.67394039744206E-17));
#7151=CARTESIAN_POINT('Origin',(0.,0.4,0.));
#7152=CARTESIAN_POINT('Origin',(0.,0.375,0.));
#7153=CARTESIAN_POINT('',(-0.35,0.35,-4.28626379701573E-17));
#7154=CARTESIAN_POINT('Origin',(0.,0.35,0.));
#7155=CARTESIAN_POINT('',(-0.325,0.375,-3.9801020972289E-17));
#7156=CARTESIAN_POINT('Origin',(0.,0.19,0.));
#7157=CARTESIAN_POINT('',(-0.35,0.03,-4.28626379701574E-17));
#7158=CARTESIAN_POINT('Origin',(0.,0.03,0.));
#7159=CARTESIAN_POINT('',(-0.35,0.19,-4.28626379701574E-17));
#7160=CARTESIAN_POINT('Origin',(0.,0.0149999999999999,0.));
#7161=CARTESIAN_POINT('',(-0.32,-3.29597460435593E-17,-3.91886975727153E-17));
#7162=CARTESIAN_POINT('Origin',(0.,0.,0.));
#7163=CARTESIAN_POINT('',(-0.335,0.0149999999999999,-4.10256677714363E-17));
#7164=CARTESIAN_POINT('Origin',(0.22,0.,0.));
#7165=CARTESIAN_POINT('',(-0.22,-6.93889390390723E-18,-2.69422295812418E-17));
#7166=CARTESIAN_POINT('Origin',(0.,0.,0.));
#7167=CARTESIAN_POINT('Origin',(0.,-0.02,0.));
#7168=CARTESIAN_POINT('',(-0.1954,-0.0492,2.39295984553393E-17));
#7169=CARTESIAN_POINT('Origin',(0.,-0.0492,0.));
#7170=CARTESIAN_POINT('',(-0.21,-0.02,-2.57175827820944E-17));
#7171=CARTESIAN_POINT('Origin',(0.,-0.8,0.));
#7172=CARTESIAN_POINT('',(-0.1954,-0.8,-2.39295984553393E-17));
#7173=CARTESIAN_POINT('',(0.,0.,0.));
#7174=CARTESIAN_POINT('Origin',(0.,0.,0.));
#7175=CARTESIAN_POINT('',(-0.42,0.16,5.14351655641888E-17));
#7176=CARTESIAN_POINT('Origin',(0.,0.16,0.));
#7177=CARTESIAN_POINT('',(-0.42,0.,5.14351655641888E-17));
#7178=CARTESIAN_POINT('',(-0.42,0.,5.14351655641888E-17));
#7179=CARTESIAN_POINT('Origin',(0.,0.,0.));
#7180=CARTESIAN_POINT('Origin',(0.,0.,0.));
#7181=CARTESIAN_POINT('',(-0.8,0.16,9.79717439317883E-17));
#7182=CARTESIAN_POINT('Origin',(0.,0.16,0.));
#7183=CARTESIAN_POINT('',(-0.8,0.,9.79717439317883E-17));
#7184=CARTESIAN_POINT('',(-0.8,0.,9.79717439317883E-17));
#7185=CARTESIAN_POINT('Origin',(0.,0.,0.));
#7186=CARTESIAN_POINT('Origin',(0.,0.16,0.));
#7187=CARTESIAN_POINT('Origin',(0.,0.,0.));
#7188=CARTESIAN_POINT('',(0.,0.,0.));
#7189=CARTESIAN_POINT('Origin',(0.,0.067277284513851,0.));
#7190=CARTESIAN_POINT('',(-0.375277674973257,0.0768195421087395,0.65));
#7191=CARTESIAN_POINT('',(0.375277674973257,0.0768195421087395,0.65));
#7192=CARTESIAN_POINT('Ctrl Pts',(-0.375277674973257,0.0768195421087395,
0.65));
#7193=CARTESIAN_POINT('Ctrl Pts',(1.66533453693773E-13,-0.0315137912242439,
0.65));
#7194=CARTESIAN_POINT('Ctrl Pts',(0.375277674973257,0.0768195421087394,
0.65));
#7195=CARTESIAN_POINT('',(-0.750555349946514,0.0768195421087394,-9.19165206894919E-17));
#7196=CARTESIAN_POINT('Ctrl Pts',(-0.750555349946514,0.0768195421087394,
-9.19165206894919E-17));
#7197=CARTESIAN_POINT('Ctrl Pts',(-0.562916512459802,-0.0315137912242434,
0.325000000000144));
#7198=CARTESIAN_POINT('Ctrl Pts',(-0.375277674973257,0.0768195421087395,
0.65));
#7199=CARTESIAN_POINT('',(-0.6175,-2.77555756156289E-17,-7.5621939847349E-17));
#7200=CARTESIAN_POINT('',(-0.734027674973257,0.067277284513851,-8.98924642641573E-17));
#7201=CARTESIAN_POINT('Origin',(0.,0.,0.));
#7202=CARTESIAN_POINT('',(-0.375277674973257,0.0768195421087395,-0.65));
#7203=CARTESIAN_POINT('Ctrl Pts',(-0.375277674973257,0.0768195421087395,
-0.65));
#7204=CARTESIAN_POINT('Ctrl Pts',(-0.562916512459968,-0.0315137912242437,
-0.324999999999856));
#7205=CARTESIAN_POINT('Ctrl Pts',(-0.750555349946514,0.0768195421087395,
-9.19165206894919E-17));
#7206=CARTESIAN_POINT('',(0.375277674973257,0.0768195421087395,-0.65));
#7207=CARTESIAN_POINT('Ctrl Pts',(0.375277674973257,0.0768195421087395,
-0.65));
#7208=CARTESIAN_POINT('Ctrl Pts',(-1.66144875635155E-13,-0.0315137912242437,
-0.65));
#7209=CARTESIAN_POINT('Ctrl Pts',(-0.375277674973257,0.0768195421087395,
-0.65));
#7210=CARTESIAN_POINT('',(0.750555349946514,0.0768195421087394,0.));
#7211=CARTESIAN_POINT('Ctrl Pts',(0.750555349946514,0.0768195421087394,
0.));
#7212=CARTESIAN_POINT('Ctrl Pts',(0.562916512459802,-0.0315137912242436,
-0.325000000000144));
#7213=CARTESIAN_POINT('Ctrl Pts',(0.375277674973257,0.0768195421087395,
-0.65));
#7214=CARTESIAN_POINT('Ctrl Pts',(0.375277674973257,0.0768195421087394,
0.65));
#7215=CARTESIAN_POINT('Ctrl Pts',(0.562916512459968,-0.0315137912242439,
0.324999999999856));
#7216=CARTESIAN_POINT('Ctrl Pts',(0.750555349946514,0.0768195421087394,
0.));
#7217=CARTESIAN_POINT('Origin',(0.,0.612722715486149,0.));
#7218=CARTESIAN_POINT('',(-0.6175,0.68,-7.5621939847349E-17));
#7219=CARTESIAN_POINT('Origin',(0.,0.68,0.));
#7220=CARTESIAN_POINT('',(-0.750555349946514,0.603180457891261,-9.19165206894919E-17));
#7221=CARTESIAN_POINT('',(-0.734027674973257,0.612722715486149,-8.98924642641573E-17));
#7222=CARTESIAN_POINT('',(-0.375277674973257,0.603180457891261,0.65));
#7223=CARTESIAN_POINT('Ctrl Pts',(-0.375277674973257,0.603180457891261,
0.65));
#7224=CARTESIAN_POINT('Ctrl Pts',(-0.562916512459968,0.711513791224243,
0.324999999999856));
#7225=CARTESIAN_POINT('Ctrl Pts',(-0.750555349946514,0.603180457891261,
-9.19165206894919E-17));
#7226=CARTESIAN_POINT('',(0.375277674973257,0.603180457891261,0.65));
#7227=CARTESIAN_POINT('Ctrl Pts',(0.375277674973257,0.603180457891261,0.65));
#7228=CARTESIAN_POINT('Ctrl Pts',(-1.66755498298699E-13,0.711513791224244,
0.65));
#7229=CARTESIAN_POINT('Ctrl Pts',(-0.375277674973257,0.603180457891261,
0.65));
#7230=CARTESIAN_POINT('',(0.750555349946514,0.603180457891261,0.));
#7231=CARTESIAN_POINT('Ctrl Pts',(0.750555349946514,0.603180457891261,0.));
#7232=CARTESIAN_POINT('Ctrl Pts',(0.562916512459802,0.711513791224244,0.325000000000144));
#7233=CARTESIAN_POINT('Ctrl Pts',(0.375277674973257,0.603180457891261,0.65));
#7234=CARTESIAN_POINT('',(0.375277674973257,0.603180457891261,-0.65));
#7235=CARTESIAN_POINT('Ctrl Pts',(0.375277674973257,0.603180457891261,-0.65));
#7236=CARTESIAN_POINT('Ctrl Pts',(0.562916512459969,0.711513791224244,-0.324999999999856));
#7237=CARTESIAN_POINT('Ctrl Pts',(0.750555349946514,0.603180457891261,0.));
#7238=CARTESIAN_POINT('',(-0.375277674973257,0.603180457891261,-0.65));
#7239=CARTESIAN_POINT('Ctrl Pts',(-0.375277674973257,0.603180457891261,
-0.65));
#7240=CARTESIAN_POINT('Ctrl Pts',(1.66422431391311E-13,0.711513791224244,
-0.65));
#7241=CARTESIAN_POINT('Ctrl Pts',(0.375277674973257,0.603180457891261,-0.65));
#7242=CARTESIAN_POINT('Ctrl Pts',(-0.750555349946514,0.603180457891261,
-9.19165206894919E-17));
#7243=CARTESIAN_POINT('Ctrl Pts',(-0.562916512459802,0.711513791224244,
-0.325000000000144));
#7244=CARTESIAN_POINT('Ctrl Pts',(-0.375277674973257,0.603180457891261,
-0.65));
#7245=CARTESIAN_POINT('Origin',(0.375277674973257,0.,-0.65));
#7246=CARTESIAN_POINT('',(-0.375277674973257,0.,-0.65));
#7247=CARTESIAN_POINT('',(0.375277674973257,0.,-0.65));
#7248=CARTESIAN_POINT('Origin',(-0.375277674973257,0.,-0.65));
#7249=CARTESIAN_POINT('',(-0.750555349946514,0.,-9.19165206894919E-17));
#7250=CARTESIAN_POINT('Origin',(-0.750555349946514,0.,-9.19165206894919E-17));
#7251=CARTESIAN_POINT('',(-0.375277674973257,0.,0.65));
#7252=CARTESIAN_POINT('Origin',(0.,0.,0.));
#7253=CARTESIAN_POINT('',(-0.338975,0.68,4.15124648740974E-17));
#7254=CARTESIAN_POINT('Origin',(0.,0.68,0.));
#7255=CARTESIAN_POINT('',(-0.338975,0.,4.15124648740974E-17));
#7256=CARTESIAN_POINT('',(-0.338975,0.,4.15124648740974E-17));
#7257=CARTESIAN_POINT('Origin',(0.,0.,0.));
#7258=CARTESIAN_POINT('Origin',(-0.375277674973257,0.,0.65));
#7259=CARTESIAN_POINT('',(0.375277674973257,0.,0.65));
#7260=CARTESIAN_POINT('Origin',(0.750555349946514,0.,0.));
#7261=CARTESIAN_POINT('',(0.750555349946514,0.,0.));
#7262=CARTESIAN_POINT('Origin',(0.375277674973257,0.,0.65));
#7263=CARTESIAN_POINT('Origin',(0.,0.68,-1.11022302462516E-16));
#7264=CARTESIAN_POINT('Origin',(0.,0.,-1.11022302462516E-16));
#7265=CARTESIAN_POINT('',(0.,0.,0.));
#7266=CARTESIAN_POINT('',(0.,0.,0.));
#7267=CARTESIAN_POINT('',(0.,0.,0.));
#7268=CARTESIAN_POINT('',(0.,0.,0.));
#7269=CARTESIAN_POINT('',(10.,-0.8,7.12132034355964));
#7270=CARTESIAN_POINT('',(10.,0.8,7.12132034355964));
#7271=CARTESIAN_POINT('',(10.,-4.,1.));
#7272=CARTESIAN_POINT('',(10.,-4.,1.16));
#7273=CARTESIAN_POINT('',(10.,-4.,7.12132034355964));
#7274=CARTESIAN_POINT('',(10.,-4.,7.28132034355964));
#7275=CARTESIAN_POINT('',(10.,4.,1.));
#7276=CARTESIAN_POINT('',(10.,4.,1.16));
#7277=CARTESIAN_POINT('',(10.,4.,7.12132034355964));
#7278=CARTESIAN_POINT('',(10.,4.,7.28132034355964));
#7279=CARTESIAN_POINT('',(0.,0.,0.));
#7280=CARTESIAN_POINT('',(0.,0.,0.));
#7281=CARTESIAN_POINT('Origin',(3.,0.,4.62132034355964));
#7282=CARTESIAN_POINT('',(17.,-1.83697019872103E-16,6.12132034355964));
#7283=CARTESIAN_POINT('Origin',(17.,0.,4.62132034355964));
#7284=CARTESIAN_POINT('',(3.,-1.83697019872103E-16,6.12132034355964));
#7285=CARTESIAN_POINT('',(3.,-1.83697019872103E-16,6.12132034355964));
#7286=CARTESIAN_POINT('Origin',(3.,0.,4.62132034355964));
#7287=CARTESIAN_POINT('Origin',(17.,0.,4.62132034355964));
#7288=CARTESIAN_POINT('Origin',(3.,0.,4.62132034355964));
#7289=CARTESIAN_POINT('',(0.,0.,0.));
#7290=CARTESIAN_POINT('',(0.,0.,0.));
#7291=CARTESIAN_POINT('',(0.,0.,0.));
#7292=CARTESIAN_POINT('',(0.,0.,0.));
#7293=UNCERTAINTY_MEASURE_WITH_UNIT(LENGTH_MEASURE(0.001),#7345,
'DISTANCE_ACCURACY_VALUE',
'Maximum model space distance between geometric entities at asserted c
onnectivities');
#7294=UNCERTAINTY_MEASURE_WITH_UNIT(LENGTH_MEASURE(0.001),#7345,
'DISTANCE_ACCURACY_VALUE',
'Maximum model space distance between geometric entities at asserted c
onnectivities');
#7295=UNCERTAINTY_MEASURE_WITH_UNIT(LENGTH_MEASURE(0.001),#7345,
'DISTANCE_ACCURACY_VALUE',
'Maximum model space distance between geometric entities at asserted c
onnectivities');
#7296=UNCERTAINTY_MEASURE_WITH_UNIT(LENGTH_MEASURE(0.001),#7345,
'DISTANCE_ACCURACY_VALUE',
'Maximum model space distance between geometric entities at asserted c
onnectivities');
#7297=UNCERTAINTY_MEASURE_WITH_UNIT(LENGTH_MEASURE(0.001),#7345,
'DISTANCE_ACCURACY_VALUE',
'Maximum model space distance between geometric entities at asserted c
onnectivities');
#7298=UNCERTAINTY_MEASURE_WITH_UNIT(LENGTH_MEASURE(0.001),#7345,
'DISTANCE_ACCURACY_VALUE',
'Maximum model space distance between geometric entities at asserted c
onnectivities');
#7299=UNCERTAINTY_MEASURE_WITH_UNIT(LENGTH_MEASURE(0.001),#7345,
'DISTANCE_ACCURACY_VALUE',
'Maximum model space distance between geometric entities at asserted c
onnectivities');
#7300=UNCERTAINTY_MEASURE_WITH_UNIT(LENGTH_MEASURE(0.001),#7345,
'DISTANCE_ACCURACY_VALUE',
'Maximum model space distance between geometric entities at asserted c
onnectivities');
#7301=UNCERTAINTY_MEASURE_WITH_UNIT(LENGTH_MEASURE(0.001),#7345,
'DISTANCE_ACCURACY_VALUE',
'Maximum model space distance between geometric entities at asserted c
onnectivities');
#7302=UNCERTAINTY_MEASURE_WITH_UNIT(LENGTH_MEASURE(0.001),#7345,
'DISTANCE_ACCURACY_VALUE',
'Maximum model space distance between geometric entities at asserted c
onnectivities');
#7303=UNCERTAINTY_MEASURE_WITH_UNIT(LENGTH_MEASURE(0.001),#7345,
'DISTANCE_ACCURACY_VALUE',
'Maximum model space distance between geometric entities at asserted c
onnectivities');
#7304=UNCERTAINTY_MEASURE_WITH_UNIT(LENGTH_MEASURE(0.001),#7345,
'DISTANCE_ACCURACY_VALUE',
'Maximum model space distance between geometric entities at asserted c
onnectivities');
#7305=UNCERTAINTY_MEASURE_WITH_UNIT(LENGTH_MEASURE(0.001),#7345,
'DISTANCE_ACCURACY_VALUE',
'Maximum model space distance between geometric entities at asserted c
onnectivities');
#7306=UNCERTAINTY_MEASURE_WITH_UNIT(LENGTH_MEASURE(0.001),#7345,
'DISTANCE_ACCURACY_VALUE',
'Maximum model space distance between geometric entities at asserted c
onnectivities');
#7307=UNCERTAINTY_MEASURE_WITH_UNIT(LENGTH_MEASURE(0.001),#7345,
'DISTANCE_ACCURACY_VALUE',
'Maximum model space distance between geometric entities at asserted c
onnectivities');
#7308=UNCERTAINTY_MEASURE_WITH_UNIT(LENGTH_MEASURE(0.001),#7345,
'DISTANCE_ACCURACY_VALUE',
'Maximum model space distance between geometric entities at asserted c
onnectivities');
#7309=UNCERTAINTY_MEASURE_WITH_UNIT(LENGTH_MEASURE(0.001),#7345,
'DISTANCE_ACCURACY_VALUE',
'Maximum model space distance between geometric entities at asserted c
onnectivities');
#7310=UNCERTAINTY_MEASURE_WITH_UNIT(LENGTH_MEASURE(0.001),#7345,
'DISTANCE_ACCURACY_VALUE',
'Maximum model space distance between geometric entities at asserted c
onnectivities');
#7311=UNCERTAINTY_MEASURE_WITH_UNIT(LENGTH_MEASURE(0.001),#7345,
'DISTANCE_ACCURACY_VALUE',
'Maximum model space distance between geometric entities at asserted c
onnectivities');
#7312=UNCERTAINTY_MEASURE_WITH_UNIT(LENGTH_MEASURE(0.001),#7345,
'DISTANCE_ACCURACY_VALUE',
'Maximum model space distance between geometric entities at asserted c
onnectivities');
#7313=UNCERTAINTY_MEASURE_WITH_UNIT(LENGTH_MEASURE(0.001),#7345,
'DISTANCE_ACCURACY_VALUE',
'Maximum model space distance between geometric entities at asserted c
onnectivities');
#7314=UNCERTAINTY_MEASURE_WITH_UNIT(LENGTH_MEASURE(0.001),#7345,
'DISTANCE_ACCURACY_VALUE',
'Maximum model space distance between geometric entities at asserted c
onnectivities');
#7315=UNCERTAINTY_MEASURE_WITH_UNIT(LENGTH_MEASURE(0.001),#7345,
'DISTANCE_ACCURACY_VALUE',
'Maximum model space distance between geometric entities at asserted c
onnectivities');
#7316=UNCERTAINTY_MEASURE_WITH_UNIT(LENGTH_MEASURE(0.001),#7345,
'DISTANCE_ACCURACY_VALUE',
'Maximum model space distance between geometric entities at asserted c
onnectivities');
#7317=UNCERTAINTY_MEASURE_WITH_UNIT(LENGTH_MEASURE(0.001),#7345,
'DISTANCE_ACCURACY_VALUE',
'Maximum model space distance between geometric entities at asserted c
onnectivities');
#7318=UNCERTAINTY_MEASURE_WITH_UNIT(LENGTH_MEASURE(0.001),#7345,
'DISTANCE_ACCURACY_VALUE',
'Maximum model space distance between geometric entities at asserted c
onnectivities');
#7319=(
GEOMETRIC_REPRESENTATION_CONTEXT(3)
GLOBAL_UNCERTAINTY_ASSIGNED_CONTEXT((#7293))
GLOBAL_UNIT_ASSIGNED_CONTEXT((#7345,#7347,#7348))
REPRESENTATION_CONTEXT('','3D')
);
#7320=(
GEOMETRIC_REPRESENTATION_CONTEXT(3)
GLOBAL_UNCERTAINTY_ASSIGNED_CONTEXT((#7294))
GLOBAL_UNIT_ASSIGNED_CONTEXT((#7345,#7347,#7348))
REPRESENTATION_CONTEXT('','3D')
);
#7321=(
GEOMETRIC_REPRESENTATION_CONTEXT(3)
GLOBAL_UNCERTAINTY_ASSIGNED_CONTEXT((#7295))
GLOBAL_UNIT_ASSIGNED_CONTEXT((#7345,#7347,#7348))
REPRESENTATION_CONTEXT('','3D')
);
#7322=(
GEOMETRIC_REPRESENTATION_CONTEXT(3)
GLOBAL_UNCERTAINTY_ASSIGNED_CONTEXT((#7296))
GLOBAL_UNIT_ASSIGNED_CONTEXT((#7345,#7347,#7348))
REPRESENTATION_CONTEXT('','3D')
);
#7323=(
GEOMETRIC_REPRESENTATION_CONTEXT(3)
GLOBAL_UNCERTAINTY_ASSIGNED_CONTEXT((#7297))
GLOBAL_UNIT_ASSIGNED_CONTEXT((#7345,#7347,#7348))
REPRESENTATION_CONTEXT('','3D')
);
#7324=(
GEOMETRIC_REPRESENTATION_CONTEXT(3)
GLOBAL_UNCERTAINTY_ASSIGNED_CONTEXT((#7298))
GLOBAL_UNIT_ASSIGNED_CONTEXT((#7345,#7347,#7348))
REPRESENTATION_CONTEXT('','3D')
);
#7325=(
GEOMETRIC_REPRESENTATION_CONTEXT(3)
GLOBAL_UNCERTAINTY_ASSIGNED_CONTEXT((#7299))
GLOBAL_UNIT_ASSIGNED_CONTEXT((#7345,#7347,#7348))
REPRESENTATION_CONTEXT('','3D')
);
#7326=(
GEOMETRIC_REPRESENTATION_CONTEXT(3)
GLOBAL_UNCERTAINTY_ASSIGNED_CONTEXT((#7300))
GLOBAL_UNIT_ASSIGNED_CONTEXT((#7345,#7347,#7348))
REPRESENTATION_CONTEXT('','3D')
);
#7327=(
GEOMETRIC_REPRESENTATION_CONTEXT(3)
GLOBAL_UNCERTAINTY_ASSIGNED_CONTEXT((#7301))
GLOBAL_UNIT_ASSIGNED_CONTEXT((#7345,#7347,#7348))
REPRESENTATION_CONTEXT('','3D')
);
#7328=(
GEOMETRIC_REPRESENTATION_CONTEXT(3)
GLOBAL_UNCERTAINTY_ASSIGNED_CONTEXT((#7302))
GLOBAL_UNIT_ASSIGNED_CONTEXT((#7345,#7347,#7348))
REPRESENTATION_CONTEXT('','3D')
);
#7329=(
GEOMETRIC_REPRESENTATION_CONTEXT(3)
GLOBAL_UNCERTAINTY_ASSIGNED_CONTEXT((#7303))
GLOBAL_UNIT_ASSIGNED_CONTEXT((#7345,#7347,#7348))
REPRESENTATION_CONTEXT('','3D')
);
#7330=(
GEOMETRIC_REPRESENTATION_CONTEXT(3)
GLOBAL_UNCERTAINTY_ASSIGNED_CONTEXT((#7304))
GLOBAL_UNIT_ASSIGNED_CONTEXT((#7345,#7347,#7348))
REPRESENTATION_CONTEXT('','3D')
);
#7331=(
GEOMETRIC_REPRESENTATION_CONTEXT(3)
GLOBAL_UNCERTAINTY_ASSIGNED_CONTEXT((#7305))
GLOBAL_UNIT_ASSIGNED_CONTEXT((#7345,#7347,#7348))
REPRESENTATION_CONTEXT('','3D')
);
#7332=(
GEOMETRIC_REPRESENTATION_CONTEXT(3)
GLOBAL_UNCERTAINTY_ASSIGNED_CONTEXT((#7306))
GLOBAL_UNIT_ASSIGNED_CONTEXT((#7345,#7347,#7348))
REPRESENTATION_CONTEXT('','3D')
);
#7333=(
GEOMETRIC_REPRESENTATION_CONTEXT(3)
GLOBAL_UNCERTAINTY_ASSIGNED_CONTEXT((#7307))
GLOBAL_UNIT_ASSIGNED_CONTEXT((#7345,#7347,#7348))
REPRESENTATION_CONTEXT('','3D')
);
#7334=(
GEOMETRIC_REPRESENTATION_CONTEXT(3)
GLOBAL_UNCERTAINTY_ASSIGNED_CONTEXT((#7308))
GLOBAL_UNIT_ASSIGNED_CONTEXT((#7345,#7347,#7348))
REPRESENTATION_CONTEXT('','3D')
);
#7335=(
GEOMETRIC_REPRESENTATION_CONTEXT(3)
GLOBAL_UNCERTAINTY_ASSIGNED_CONTEXT((#7309))
GLOBAL_UNIT_ASSIGNED_CONTEXT((#7345,#7347,#7348))
REPRESENTATION_CONTEXT('','3D')
);
#7336=(
GEOMETRIC_REPRESENTATION_CONTEXT(3)
GLOBAL_UNCERTAINTY_ASSIGNED_CONTEXT((#7310))
GLOBAL_UNIT_ASSIGNED_CONTEXT((#7345,#7347,#7348))
REPRESENTATION_CONTEXT('','3D')
);
#7337=(
GEOMETRIC_REPRESENTATION_CONTEXT(3)
GLOBAL_UNCERTAINTY_ASSIGNED_CONTEXT((#7311))
GLOBAL_UNIT_ASSIGNED_CONTEXT((#7345,#7347,#7348))
REPRESENTATION_CONTEXT('','3D')
);
#7338=(
GEOMETRIC_REPRESENTATION_CONTEXT(3)
GLOBAL_UNCERTAINTY_ASSIGNED_CONTEXT((#7312))
GLOBAL_UNIT_ASSIGNED_CONTEXT((#7345,#7347,#7348))
REPRESENTATION_CONTEXT('','3D')
);
#7339=(
GEOMETRIC_REPRESENTATION_CONTEXT(3)
GLOBAL_UNCERTAINTY_ASSIGNED_CONTEXT((#7313))
GLOBAL_UNIT_ASSIGNED_CONTEXT((#7345,#7347,#7348))
REPRESENTATION_CONTEXT('','3D')
);
#7340=(
GEOMETRIC_REPRESENTATION_CONTEXT(3)
GLOBAL_UNCERTAINTY_ASSIGNED_CONTEXT((#7314))
GLOBAL_UNIT_ASSIGNED_CONTEXT((#7345,#7347,#7348))
REPRESENTATION_CONTEXT('','3D')
);
#7341=(
GEOMETRIC_REPRESENTATION_CONTEXT(3)
GLOBAL_UNCERTAINTY_ASSIGNED_CONTEXT((#7315))
GLOBAL_UNIT_ASSIGNED_CONTEXT((#7345,#7347,#7348))
REPRESENTATION_CONTEXT('','3D')
);
#7342=(
GEOMETRIC_REPRESENTATION_CONTEXT(3)
GLOBAL_UNCERTAINTY_ASSIGNED_CONTEXT((#7316))
GLOBAL_UNIT_ASSIGNED_CONTEXT((#7345,#7347,#7348))
REPRESENTATION_CONTEXT('','3D')
);
#7343=(
GEOMETRIC_REPRESENTATION_CONTEXT(3)
GLOBAL_UNCERTAINTY_ASSIGNED_CONTEXT((#7317))
GLOBAL_UNIT_ASSIGNED_CONTEXT((#7345,#7347,#7348))
REPRESENTATION_CONTEXT('','3D')
);
#7344=(
GEOMETRIC_REPRESENTATION_CONTEXT(3)
GLOBAL_UNCERTAINTY_ASSIGNED_CONTEXT((#7318))
GLOBAL_UNIT_ASSIGNED_CONTEXT((#7345,#7347,#7348))
REPRESENTATION_CONTEXT('','3D')
);
#7345=(
LENGTH_UNIT()
NAMED_UNIT(*)
SI_UNIT(.CENTI.,.METRE.)
);
#7346=(
LENGTH_UNIT()
NAMED_UNIT(*)
SI_UNIT($,.METRE.)
);
#7347=(
NAMED_UNIT(*)
PLANE_ANGLE_UNIT()
SI_UNIT($,.RADIAN.)
);
#7348=(
NAMED_UNIT(*)
SI_UNIT($,.STERADIAN.)
SOLID_ANGLE_UNIT()
);
#7349=SHAPE_DEFINITION_REPRESENTATION(#7374,#7440);
#7350=SHAPE_DEFINITION_REPRESENTATION(#7375,#7441);
#7351=SHAPE_DEFINITION_REPRESENTATION(#7376,#7442);
#7352=SHAPE_DEFINITION_REPRESENTATION(#7377,#7443);
#7353=SHAPE_DEFINITION_REPRESENTATION(#7378,#7444);
#7354=SHAPE_DEFINITION_REPRESENTATION(#7379,#7445);
#7355=SHAPE_DEFINITION_REPRESENTATION(#7380,#7446);
#7356=SHAPE_DEFINITION_REPRESENTATION(#7381,#7447);
#7357=SHAPE_DEFINITION_REPRESENTATION(#7382,#7448);
#7358=SHAPE_DEFINITION_REPRESENTATION(#7383,#7449);
#7359=SHAPE_DEFINITION_REPRESENTATION(#7384,#7450);
#7360=SHAPE_DEFINITION_REPRESENTATION(#7385,#7451);
#7361=SHAPE_DEFINITION_REPRESENTATION(#7386,#7452);
#7362=SHAPE_DEFINITION_REPRESENTATION(#7387,#7453);
#7363=SHAPE_DEFINITION_REPRESENTATION(#7388,#7454);
#7364=SHAPE_DEFINITION_REPRESENTATION(#7412,#7455);
#7365=SHAPE_DEFINITION_REPRESENTATION(#7413,#7456);
#7366=SHAPE_DEFINITION_REPRESENTATION(#7414,#7457);
#7367=SHAPE_DEFINITION_REPRESENTATION(#7415,#7458);
#7368=SHAPE_DEFINITION_REPRESENTATION(#7416,#7459);
#7369=SHAPE_DEFINITION_REPRESENTATION(#7417,#7460);
#7370=SHAPE_DEFINITION_REPRESENTATION(#7418,#7461);
#7371=SHAPE_DEFINITION_REPRESENTATION(#7419,#7462);
#7372=SHAPE_DEFINITION_REPRESENTATION(#7434,#7463);
#7373=SHAPE_DEFINITION_REPRESENTATION(#7435,#7464);
#7374=PRODUCT_DEFINITION_SHAPE('',$,#7466);
#7375=PRODUCT_DEFINITION_SHAPE('',$,#7467);
#7376=PRODUCT_DEFINITION_SHAPE('',$,#7468);
#7377=PRODUCT_DEFINITION_SHAPE('',$,#7469);
#7378=PRODUCT_DEFINITION_SHAPE('',$,#7470);
#7379=PRODUCT_DEFINITION_SHAPE('',$,#7471);
#7380=PRODUCT_DEFINITION_SHAPE('',$,#7472);
#7381=PRODUCT_DEFINITION_SHAPE('',$,#7473);
#7382=PRODUCT_DEFINITION_SHAPE('',$,#7474);
#7383=PRODUCT_DEFINITION_SHAPE('',$,#7475);
#7384=PRODUCT_DEFINITION_SHAPE('',$,#7476);
#7385=PRODUCT_DEFINITION_SHAPE('',$,#7477);
#7386=PRODUCT_DEFINITION_SHAPE('',$,#7478);
#7387=PRODUCT_DEFINITION_SHAPE('',$,#7479);
#7388=PRODUCT_DEFINITION_SHAPE('',$,#7480);
#7389=PRODUCT_DEFINITION_SHAPE($,$,#134);
#7390=PRODUCT_DEFINITION_SHAPE($,$,#135);
#7391=PRODUCT_DEFINITION_SHAPE($,$,#136);
#7392=PRODUCT_DEFINITION_SHAPE($,$,#137);
#7393=PRODUCT_DEFINITION_SHAPE($,$,#138);
#7394=PRODUCT_DEFINITION_SHAPE($,$,#139);
#7395=PRODUCT_DEFINITION_SHAPE($,$,#140);
#7396=PRODUCT_DEFINITION_SHAPE($,$,#141);
#7397=PRODUCT_DEFINITION_SHAPE($,$,#142);
#7398=PRODUCT_DEFINITION_SHAPE($,$,#143);
#7399=PRODUCT_DEFINITION_SHAPE($,$,#144);
#7400=PRODUCT_DEFINITION_SHAPE($,$,#145);
#7401=PRODUCT_DEFINITION_SHAPE($,$,#146);
#7402=PRODUCT_DEFINITION_SHAPE($,$,#147);
#7403=PRODUCT_DEFINITION_SHAPE($,$,#148);
#7404=PRODUCT_DEFINITION_SHAPE($,$,#149);
#7405=PRODUCT_DEFINITION_SHAPE($,$,#150);
#7406=PRODUCT_DEFINITION_SHAPE($,$,#151);
#7407=PRODUCT_DEFINITION_SHAPE($,$,#152);
#7408=PRODUCT_DEFINITION_SHAPE($,$,#153);
#7409=PRODUCT_DEFINITION_SHAPE($,$,#154);
#7410=PRODUCT_DEFINITION_SHAPE($,$,#155);
#7411=PRODUCT_DEFINITION_SHAPE($,$,#156);
#7412=PRODUCT_DEFINITION_SHAPE('',$,#7481);
#7413=PRODUCT_DEFINITION_SHAPE('',$,#7482);
#7414=PRODUCT_DEFINITION_SHAPE('',$,#7483);
#7415=PRODUCT_DEFINITION_SHAPE('',$,#7484);
#7416=PRODUCT_DEFINITION_SHAPE('',$,#7485);
#7417=PRODUCT_DEFINITION_SHAPE('',$,#7486);
#7418=PRODUCT_DEFINITION_SHAPE('',$,#7487);
#7419=PRODUCT_DEFINITION_SHAPE('',$,#7488);
#7420=PRODUCT_DEFINITION_SHAPE($,$,#157);
#7421=PRODUCT_DEFINITION_SHAPE($,$,#158);
#7422=PRODUCT_DEFINITION_SHAPE($,$,#159);
#7423=PRODUCT_DEFINITION_SHAPE($,$,#160);
#7424=PRODUCT_DEFINITION_SHAPE($,$,#161);
#7425=PRODUCT_DEFINITION_SHAPE($,$,#162);
#7426=PRODUCT_DEFINITION_SHAPE($,$,#163);
#7427=PRODUCT_DEFINITION_SHAPE($,$,#164);
#7428=PRODUCT_DEFINITION_SHAPE($,$,#165);
#7429=PRODUCT_DEFINITION_SHAPE($,$,#166);
#7430=PRODUCT_DEFINITION_SHAPE($,$,#167);
#7431=PRODUCT_DEFINITION_SHAPE($,$,#168);
#7432=PRODUCT_DEFINITION_SHAPE($,$,#169);
#7433=PRODUCT_DEFINITION_SHAPE($,$,#170);
#7434=PRODUCT_DEFINITION_SHAPE('',$,#7489);
#7435=PRODUCT_DEFINITION_SHAPE('',$,#7490);
#7436=PRODUCT_DEFINITION_SHAPE($,$,#171);
#7437=PRODUCT_DEFINITION_SHAPE($,$,#172);
#7438=PRODUCT_DEFINITION_SHAPE($,$,#173);
#7439=PRODUCT_DEFINITION_SHAPE($,$,#174);
#7440=SHAPE_REPRESENTATION('',(#4404,#4840,#4841,#4842),#7319);
#7441=SHAPE_REPRESENTATION('',(#4405,#4697,#4698,#4699,#4700,#4701,#4702,
#4703,#4704,#4705,#4706,#4707,#4708,#4709,#4710,#4711,#4712,#4713,#4714,
#4715,#4716,#4717,#4718,#4719),#7320);
#7442=SHAPE_REPRESENTATION('',(#4406),#7321);
#7443=SHAPE_REPRESENTATION('',(#4459),#7322);
#7444=SHAPE_REPRESENTATION('',(#4472),#7323);
#7445=SHAPE_REPRESENTATION('',(#4479),#7324);
#7446=SHAPE_REPRESENTATION('',(#4492),#7325);
#7447=SHAPE_REPRESENTATION('',(#4499),#7326);
#7448=SHAPE_REPRESENTATION('',(#4538),#7327);
#7449=SHAPE_REPRESENTATION('',(#4577),#7328);
#7450=SHAPE_REPRESENTATION('',(#4609),#7329);
#7451=SHAPE_REPRESENTATION('',(#4620),#7330);
#7452=SHAPE_REPRESENTATION('',(#4646),#7331);
#7453=SHAPE_REPRESENTATION('',(#4672),#7332);
#7454=SHAPE_REPRESENTATION('',(#4681),#7333);
#7455=SHAPE_REPRESENTATION('',(#4720,#4818,#4819,#4820,#4821,#4822,#4823,
#4824,#4825,#4826,#4827,#4828,#4829,#4830,#4831),#7334);
#7456=SHAPE_REPRESENTATION('',(#4721),#7335);
#7457=SHAPE_REPRESENTATION('',(#4740),#7336);
#7458=SHAPE_REPRESENTATION('',(#4757),#7337);
#7459=SHAPE_REPRESENTATION('',(#4763),#7338);
#7460=SHAPE_REPRESENTATION('',(#4769),#7339);
#7461=SHAPE_REPRESENTATION('',(#4793),#7340);
#7462=SHAPE_REPRESENTATION('',(#4802),#7341);
#7463=SHAPE_REPRESENTATION('',(#4832,#4839),#7342);
#7464=SHAPE_REPRESENTATION('',(#4833),#7343);
#7465=PRODUCT_DEFINITION_CONTEXT('part definition',#7542,'design');
#7466=PRODUCT_DEFINITION('PAT-116','PAT-116',#7491,#7465);
#7467=PRODUCT_DEFINITION('Located fixture','Located fixture',#7492,#7465);
#7468=PRODUCT_DEFINITION('Base','Base',#7493,#7465);
#7469=PRODUCT_DEFINITION('Foot','Foot',#7494,#7465);
#7470=PRODUCT_DEFINITION('Bonded foot pad','Bonded foot pad',#7495,#7465);
#7471=PRODUCT_DEFINITION('Foot (1)','Foot (1)',#7496,#7465);
#7472=PRODUCT_DEFINITION('Bonded foot pad (1)','Bonded foot pad (1)',#7497,
#7465);
#7473=PRODUCT_DEFINITION('V block','V block',#7498,#7465);
#7474=PRODUCT_DEFINITION('V block (1)','V block (1)',#7499,#7465);
#7475=PRODUCT_DEFINITION('End stop','End stop',#7500,#7465);
#7476=PRODUCT_DEFINITION('Key 6x6x20','Key 6x6x20',#7501,#7465);
#7477=PRODUCT_DEFINITION('Cap Screw - M6x25','Cap Screw - M6x25',#7502,
#7465);
#7478=PRODUCT_DEFINITION('Cap Screw - M5x20','Cap Screw - M5x20',#7503,
#7465);
#7479=PRODUCT_DEFINITION('Flat Washer - M5','Flat Washer - M5',#7504,#7465);
#7480=PRODUCT_DEFINITION('Hex Nut - M5','Hex Nut - M5',#7505,#7465);
#7481=PRODUCT_DEFINITION('Strap and studs','Strap and studs',#7506,#7465);
#7482=PRODUCT_DEFINITION('Strap','Strap',#7507,#7465);
#7483=PRODUCT_DEFINITION('Replaceable contact pad',
'Replaceable contact pad',#7508,#7465);
#7484=PRODUCT_DEFINITION('M8 clamp stud','M8 clamp stud',#7509,#7465);
#7485=PRODUCT_DEFINITION('M8 clamp stud (1)','M8 clamp stud (1)',#7510,#7465);
#7486=PRODUCT_DEFINITION('M4x10 Cap Screw','M4x10 Cap Screw',#7511,#7465);
#7487=PRODUCT_DEFINITION('Flat Washer - M8','Flat Washer - M8',#7512,#7465);
#7488=PRODUCT_DEFINITION('Hex Nut - M8','Hex Nut - M8',#7513,#7465);
#7489=PRODUCT_DEFINITION('Example round stock (1)',
'Example round stock (1)',#7514,#7465);
#7490=PRODUCT_DEFINITION('Example round stock','Example round stock',
#7515,#7465);
#7491=PRODUCT_DEFINITION_FORMATION('',$,#7544);
#7492=PRODUCT_DEFINITION_FORMATION('',$,#7545);
#7493=PRODUCT_DEFINITION_FORMATION('',$,#7546);
#7494=PRODUCT_DEFINITION_FORMATION('',$,#7547);
#7495=PRODUCT_DEFINITION_FORMATION('',$,#7548);
#7496=PRODUCT_DEFINITION_FORMATION('',$,#7549);
#7497=PRODUCT_DEFINITION_FORMATION('',$,#7550);
#7498=PRODUCT_DEFINITION_FORMATION('',$,#7551);
#7499=PRODUCT_DEFINITION_FORMATION('',$,#7552);
#7500=PRODUCT_DEFINITION_FORMATION('',$,#7553);
#7501=PRODUCT_DEFINITION_FORMATION('',$,#7554);
#7502=PRODUCT_DEFINITION_FORMATION('',$,#7555);
#7503=PRODUCT_DEFINITION_FORMATION('',$,#7556);
#7504=PRODUCT_DEFINITION_FORMATION('',$,#7557);
#7505=PRODUCT_DEFINITION_FORMATION('',$,#7558);
#7506=PRODUCT_DEFINITION_FORMATION('',$,#7559);
#7507=PRODUCT_DEFINITION_FORMATION('',$,#7560);
#7508=PRODUCT_DEFINITION_FORMATION('',$,#7561);
#7509=PRODUCT_DEFINITION_FORMATION('',$,#7562);
#7510=PRODUCT_DEFINITION_FORMATION('',$,#7563);
#7511=PRODUCT_DEFINITION_FORMATION('',$,#7564);
#7512=PRODUCT_DEFINITION_FORMATION('',$,#7565);
#7513=PRODUCT_DEFINITION_FORMATION('',$,#7566);
#7514=PRODUCT_DEFINITION_FORMATION('',$,#7567);
#7515=PRODUCT_DEFINITION_FORMATION('',$,#7568);
#7516=PRODUCT_RELATED_PRODUCT_CATEGORY('PAT-116','PAT-116',(#7544));
#7517=PRODUCT_RELATED_PRODUCT_CATEGORY('Located fixture',
'Located fixture',(#7545));
#7518=PRODUCT_RELATED_PRODUCT_CATEGORY('Base','Base',(#7546));
#7519=PRODUCT_RELATED_PRODUCT_CATEGORY('Foot','Foot',(#7547));
#7520=PRODUCT_RELATED_PRODUCT_CATEGORY('Bonded foot pad',
'Bonded foot pad',(#7548));
#7521=PRODUCT_RELATED_PRODUCT_CATEGORY('Foot (1)','Foot (1)',(#7549));
#7522=PRODUCT_RELATED_PRODUCT_CATEGORY('Bonded foot pad (1)',
'Bonded foot pad (1)',(#7550));
#7523=PRODUCT_RELATED_PRODUCT_CATEGORY('V block','V block',(#7551));
#7524=PRODUCT_RELATED_PRODUCT_CATEGORY('V block (1)','V block (1)',(#7552));
#7525=PRODUCT_RELATED_PRODUCT_CATEGORY('End stop','End stop',(#7553));
#7526=PRODUCT_RELATED_PRODUCT_CATEGORY('Key 6x6x20','Key 6x6x20',(#7554));
#7527=PRODUCT_RELATED_PRODUCT_CATEGORY('Cap Screw - M6x25',
'Cap Screw - M6x25',(#7555));
#7528=PRODUCT_RELATED_PRODUCT_CATEGORY('Cap Screw - M5x20',
'Cap Screw - M5x20',(#7556));
#7529=PRODUCT_RELATED_PRODUCT_CATEGORY('Flat Washer - M5',
'Flat Washer - M5',(#7557));
#7530=PRODUCT_RELATED_PRODUCT_CATEGORY('Hex Nut - M5','Hex Nut - M5',(#7558));
#7531=PRODUCT_RELATED_PRODUCT_CATEGORY('Strap and studs',
'Strap and studs',(#7559));
#7532=PRODUCT_RELATED_PRODUCT_CATEGORY('Strap','Strap',(#7560));
#7533=PRODUCT_RELATED_PRODUCT_CATEGORY('Replaceable contact pad',
'Replaceable contact pad',(#7561));
#7534=PRODUCT_RELATED_PRODUCT_CATEGORY('M8 clamp stud','M8 clamp stud',
(#7562));
#7535=PRODUCT_RELATED_PRODUCT_CATEGORY('M8 clamp stud (1)',
'M8 clamp stud (1)',(#7563));
#7536=PRODUCT_RELATED_PRODUCT_CATEGORY('M4x10 Cap Screw',
'M4x10 Cap Screw',(#7564));
#7537=PRODUCT_RELATED_PRODUCT_CATEGORY('Flat Washer - M8',
'Flat Washer - M8',(#7565));
#7538=PRODUCT_RELATED_PRODUCT_CATEGORY('Hex Nut - M8','Hex Nut - M8',(#7566));
#7539=PRODUCT_RELATED_PRODUCT_CATEGORY('Example round stock (1)',
'Example round stock (1)',(#7567));
#7540=PRODUCT_RELATED_PRODUCT_CATEGORY('Example round stock',
'Example round stock',(#7568));
#7541=APPLICATION_PROTOCOL_DEFINITION('international standard',
'automotive_design',2009,#7542);
#7542=APPLICATION_CONTEXT(
'Core Data for Automotive Mechanical Design Process');
#7543=PRODUCT_CONTEXT('part definition',#7542,'mechanical');
#7544=PRODUCT('PAT-116','PAT-116',
'PAT-116',(#7543));
#7545=PRODUCT('Located fixture','Located fixture','Located fixture',(#7543));
#7546=PRODUCT('Base','Base','Base',(#7543));
#7547=PRODUCT('Foot','Foot','Foot',(#7543));
#7548=PRODUCT('Bonded foot pad','Bonded foot pad','Bonded foot pad',(#7543));
#7549=PRODUCT('Foot (1)','Foot (1)','Foot (1)',(#7543));
#7550=PRODUCT('Bonded foot pad (1)','Bonded foot pad (1)',
'Bonded foot pad (1)',(#7543));
#7551=PRODUCT('V block','V block','V block',(#7543));
#7552=PRODUCT('V block (1)','V block (1)','V block (1)',(#7543));
#7553=PRODUCT('End stop','End stop','End stop',(#7543));
#7554=PRODUCT('Key 6x6x20','Key 6x6x20','Key 6x6x20',(#7543));
#7555=PRODUCT('Cap Screw - M6x25','Cap Screw - M6x25',
'Cap Screw - M6x25',(#7543));
#7556=PRODUCT('Cap Screw - M5x20','Cap Screw - M5x20',
'Cap Screw - M5x20',(#7543));
#7557=PRODUCT('Flat Washer - M5','Flat Washer - M5','Flat Washer - M5',
(#7543));
#7558=PRODUCT('Hex Nut - M5','Hex Nut - M5','Hex Nut - M5',(#7543));
#7559=PRODUCT('Strap and studs','Strap and studs','Strap and studs',(#7543));
#7560=PRODUCT('Strap','Strap','Strap',(#7543));
#7561=PRODUCT('Replaceable contact pad','Replaceable contact pad',
'Replaceable contact pad',(#7543));
#7562=PRODUCT('M8 clamp stud','M8 clamp stud','M8 clamp stud',(#7543));
#7563=PRODUCT('M8 clamp stud (1)','M8 clamp stud (1)','M8 clamp stud (1)',(#7543));
#7564=PRODUCT('M4x10 Cap Screw','M4x10 Cap Screw','M4x10 Cap Screw',(#7543));
#7565=PRODUCT('Flat Washer - M8','Flat Washer - M8','Flat Washer - M8',
(#7543));
#7566=PRODUCT('Hex Nut - M8','Hex Nut - M8','Hex Nut - M8',(#7543));
#7567=PRODUCT('Example round stock (1)','Example round stock (1)',
'Example round stock (1)',(#7543));
#7568=PRODUCT('Example round stock','Example round stock',
'Example round stock',(#7543));
#7569=PRESENTATION_STYLE_ASSIGNMENT((#7574));
#7570=PRESENTATION_STYLE_ASSIGNMENT((#7575));
#7571=PRESENTATION_STYLE_ASSIGNMENT((#7576));
#7572=PRESENTATION_STYLE_ASSIGNMENT((#7577));
#7573=PRESENTATION_STYLE_ASSIGNMENT((#7578));
#7574=SURFACE_STYLE_USAGE(.BOTH.,#7579);
#7575=SURFACE_STYLE_USAGE(.BOTH.,#7580);
#7576=SURFACE_STYLE_USAGE(.BOTH.,#7581);
#7577=SURFACE_STYLE_USAGE(.BOTH.,#7582);
#7578=SURFACE_STYLE_USAGE(.BOTH.,#7583);
#7579=SURFACE_SIDE_STYLE('',(#7584));
#7580=SURFACE_SIDE_STYLE('',(#7585));
#7581=SURFACE_SIDE_STYLE('',(#7586));
#7582=SURFACE_SIDE_STYLE('',(#7587));
#7583=SURFACE_SIDE_STYLE('',(#7588));
#7584=SURFACE_STYLE_FILL_AREA(#7589);
#7585=SURFACE_STYLE_FILL_AREA(#7590);
#7586=SURFACE_STYLE_FILL_AREA(#7591);
#7587=SURFACE_STYLE_FILL_AREA(#7592);
#7588=SURFACE_STYLE_FILL_AREA(#7593);
#7589=FILL_AREA_STYLE('Steel - Satin',(#7594));
#7590=FILL_AREA_STYLE('CAD Library Painted - Deep blue',(#7595));
#7591=FILL_AREA_STYLE('CAD Library Painted - Graphite',(#7596));
#7592=FILL_AREA_STYLE('CAD Library Painted - Engineering blue',(#7597));
#7593=FILL_AREA_STYLE('CAD Library Painted - Steel gray',(#7598));
#7594=FILL_AREA_STYLE_COLOUR('Steel - Satin',#7599);
#7595=FILL_AREA_STYLE_COLOUR('CAD Library Painted - Deep blue',#7600);
#7596=FILL_AREA_STYLE_COLOUR('CAD Library Painted - Graphite',#7601);
#7597=FILL_AREA_STYLE_COLOUR('CAD Library Painted - Engineering blue',#7602);
#7598=FILL_AREA_STYLE_COLOUR('CAD Library Painted - Steel gray',#7603);
#7599=COLOUR_RGB('Steel - Satin',0.627450980392157,0.627450980392157,0.627450980392157);
#7600=COLOUR_RGB('CAD Library Painted - Deep blue',0.0784313725490196,0.203921568627451,
0.349019607843137);
#7601=COLOUR_RGB('CAD Library Painted - Graphite',0.168627450980392,0.192156862745098,
0.231372549019608);
#7602=COLOUR_RGB('CAD Library Painted - Engineering blue',0.12156862745098,
0.356862745098039,0.6);
#7603=COLOUR_RGB('CAD Library Painted - Steel gray',0.592156862745098,0.631372549019608,
0.67843137254902);
#7604=COLOUR_RGB('Dark Blue',0.08,0.2,0.34);
#7605=FILL_AREA_STYLE_COLOUR('',#7604);
#7606=FILL_AREA_STYLE('',(#7605));
#7607=SURFACE_STYLE_FILL_AREA(#7606);
#7608=SURFACE_SIDE_STYLE('',(#7607));
#7609=SURFACE_STYLE_USAGE(.BOTH.,#7608);
#7610=PRESENTATION_STYLE_ASSIGNMENT((#7609));
#7611=COLOUR_RGB('Light Blue',0.38,0.62,0.78);
#7612=FILL_AREA_STYLE_COLOUR('',#7611);
#7613=FILL_AREA_STYLE('',(#7612));
#7614=SURFACE_STYLE_FILL_AREA(#7613);
#7615=SURFACE_SIDE_STYLE('',(#7614));
#7616=SURFACE_STYLE_USAGE(.BOTH.,#7615);
#7617=PRESENTATION_STYLE_ASSIGNMENT((#7616));
#7618=COLOUR_RGB('Sky Blue',0.24,0.69,0.87);
#7619=FILL_AREA_STYLE_COLOUR('',#7618);
#7620=FILL_AREA_STYLE('',(#7619));
#7621=SURFACE_STYLE_FILL_AREA(#7620);
#7622=SURFACE_SIDE_STYLE('',(#7621));
#7623=SURFACE_STYLE_USAGE(.BOTH.,#7622);
#7624=PRESENTATION_STYLE_ASSIGNMENT((#7623));
#7625=COLOUR_RGB('Grey',0.48,0.52,0.57);
#7626=FILL_AREA_STYLE_COLOUR('',#7625);
#7627=FILL_AREA_STYLE('',(#7626));
#7628=SURFACE_STYLE_FILL_AREA(#7627);
#7629=SURFACE_SIDE_STYLE('',(#7628));
#7630=SURFACE_STYLE_USAGE(.BOTH.,#7629);
#7631=PRESENTATION_STYLE_ASSIGNMENT((#7630));
#7632=COLOUR_RGB('Black',0.12,0.14,0.17);
#7633=FILL_AREA_STYLE_COLOUR('',#7632);
#7634=FILL_AREA_STYLE('',(#7633));
#7635=SURFACE_STYLE_FILL_AREA(#7634);
#7636=SURFACE_SIDE_STYLE('',(#7635));
#7637=SURFACE_STYLE_USAGE(.BOTH.,#7636);
#7638=PRESENTATION_STYLE_ASSIGNMENT((#7637));
#7639=COLOUR_RGB('Off White',0.89,0.88,0.83);
#7640=FILL_AREA_STYLE_COLOUR('',#7639);
#7641=FILL_AREA_STYLE('',(#7640));
#7642=SURFACE_STYLE_FILL_AREA(#7641);
#7643=SURFACE_SIDE_STYLE('',(#7642));
#7644=SURFACE_STYLE_USAGE(.BOTH.,#7643);
#7645=PRESENTATION_STYLE_ASSIGNMENT((#7644));
ENDSEC;
END-ISO-10303-21;
